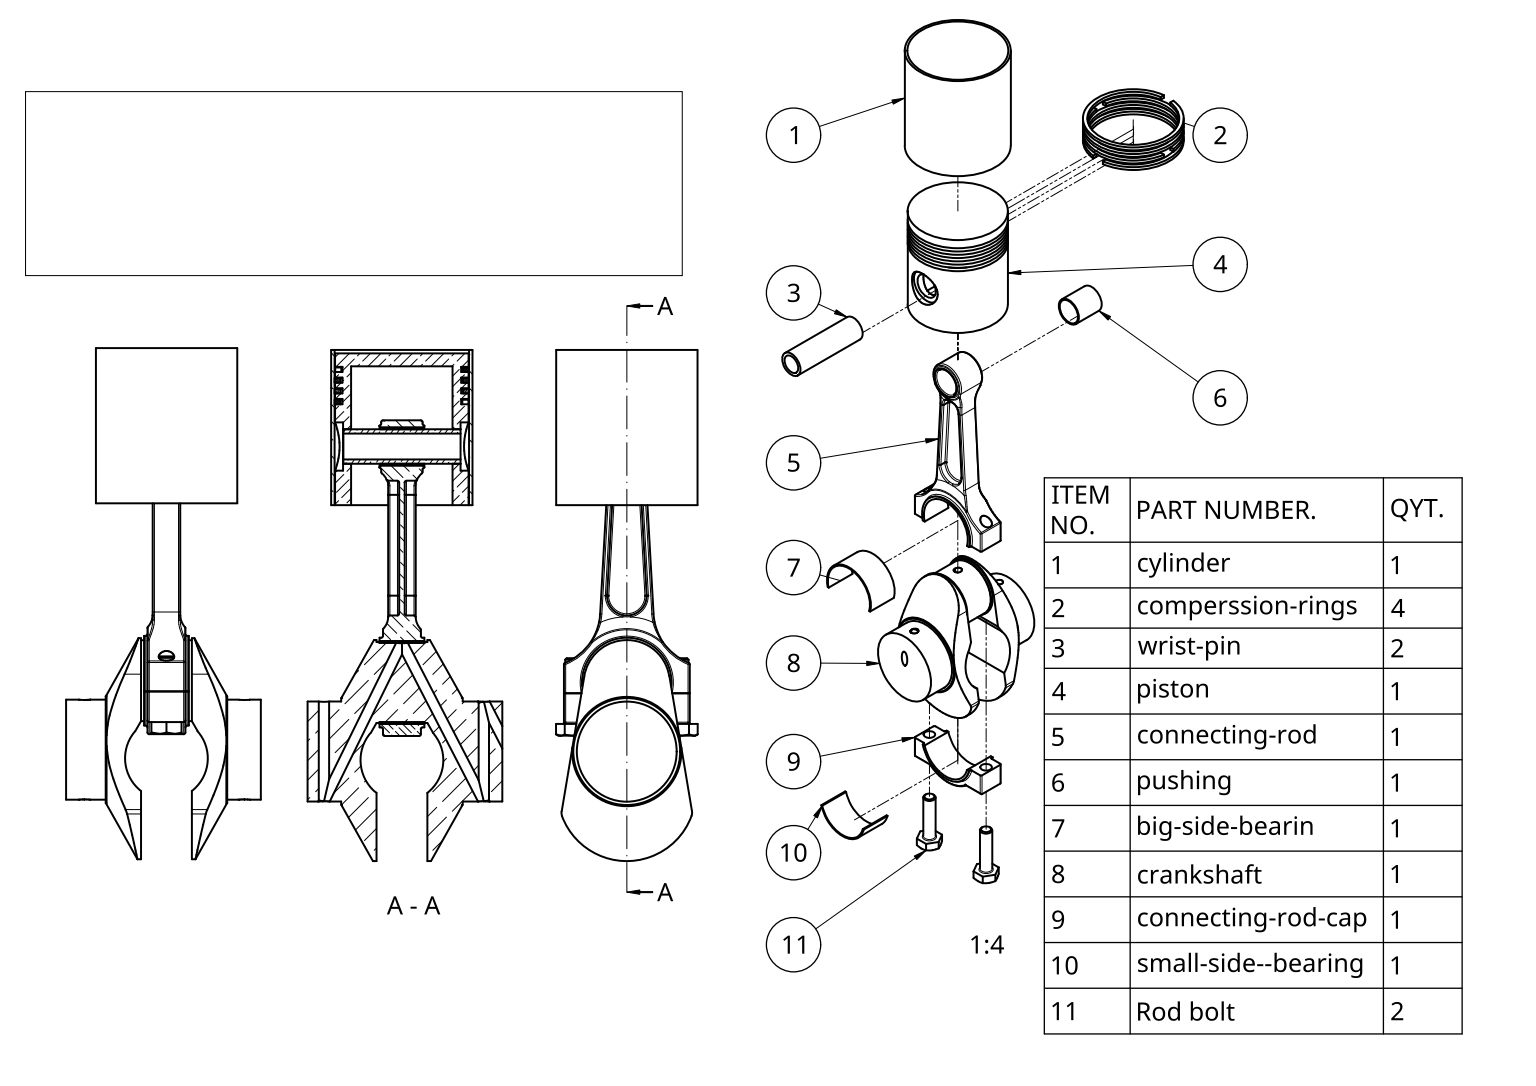
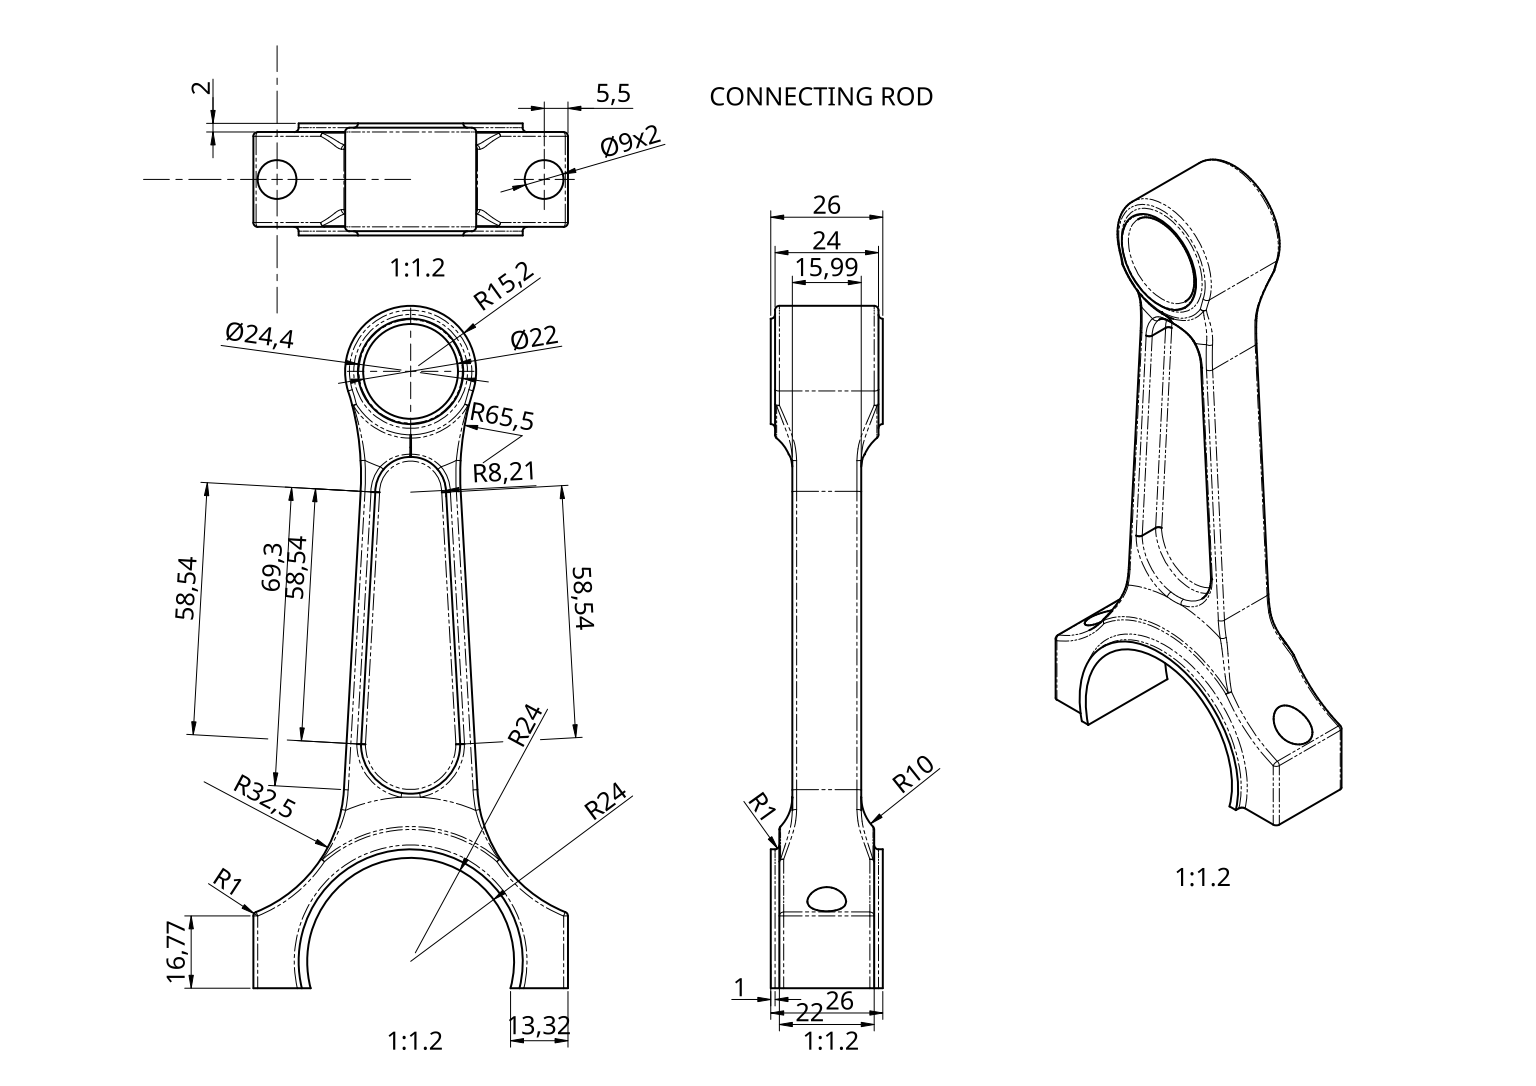
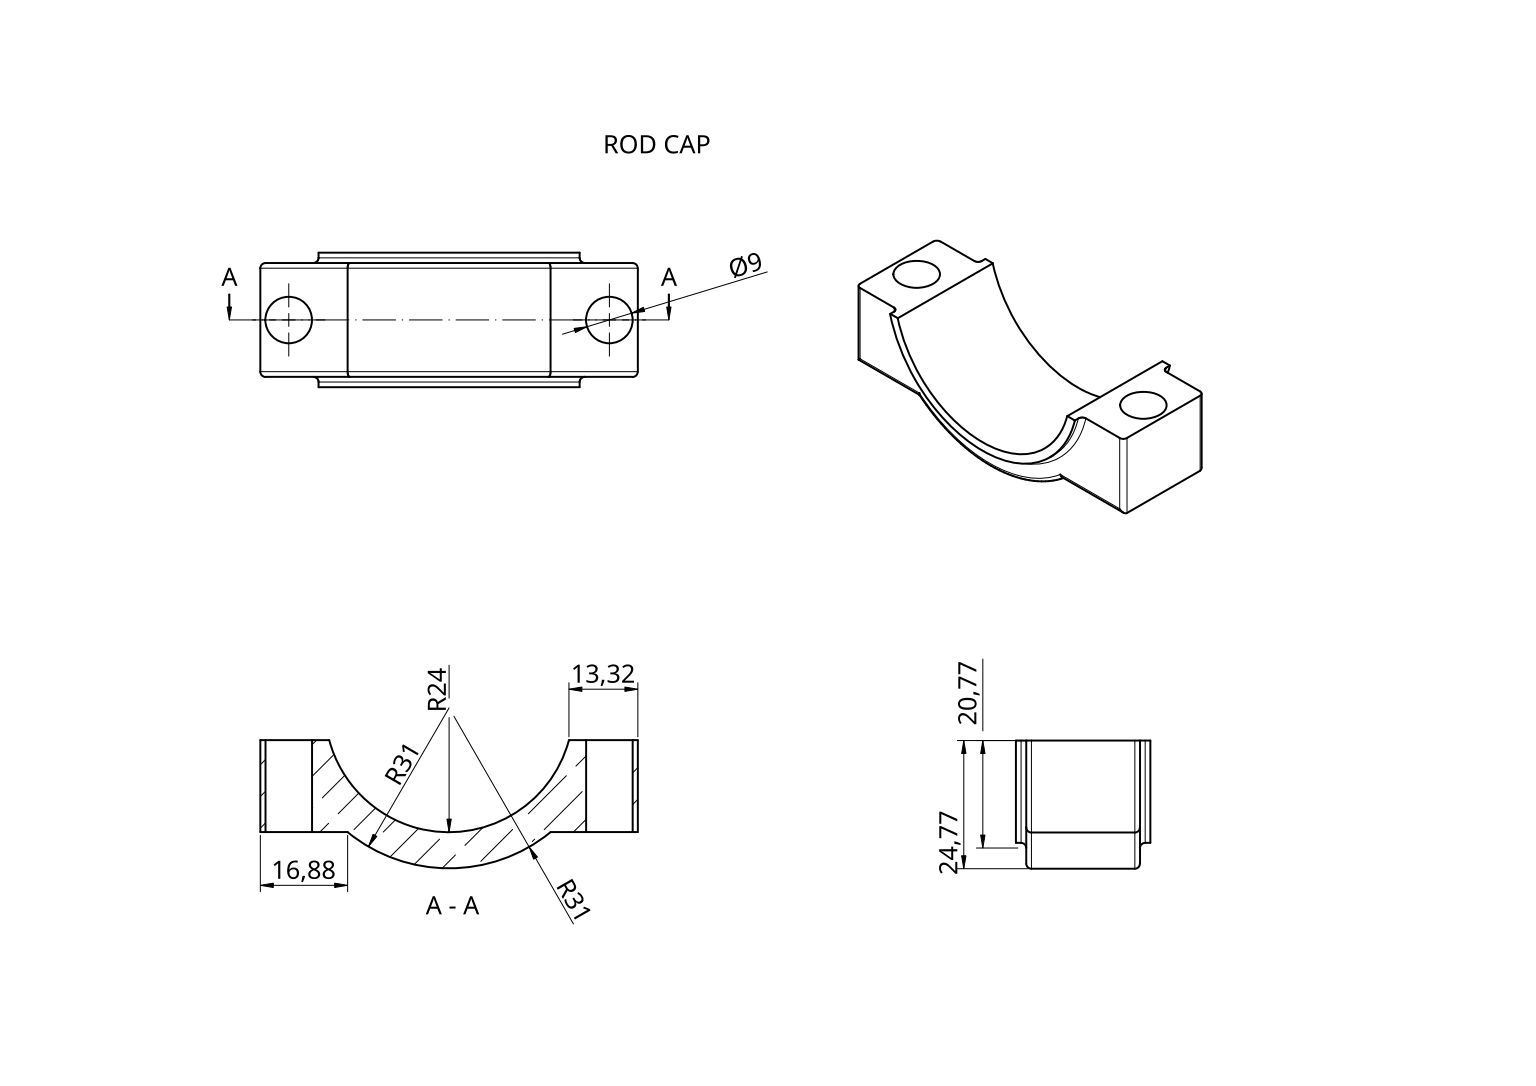
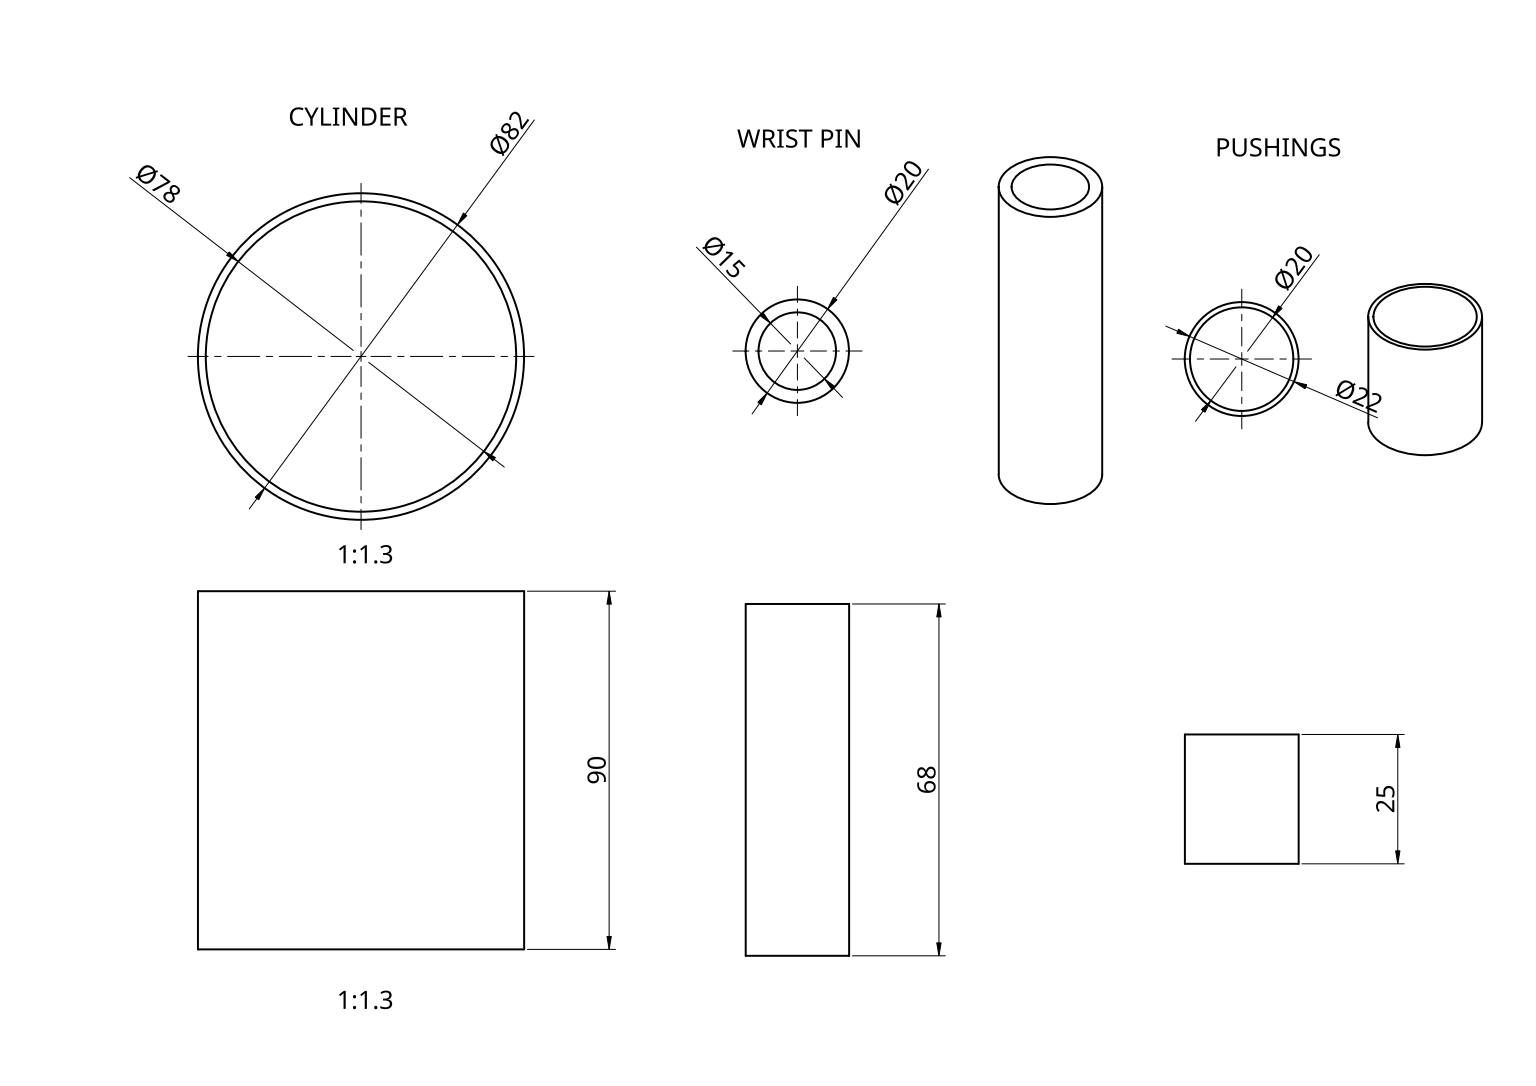
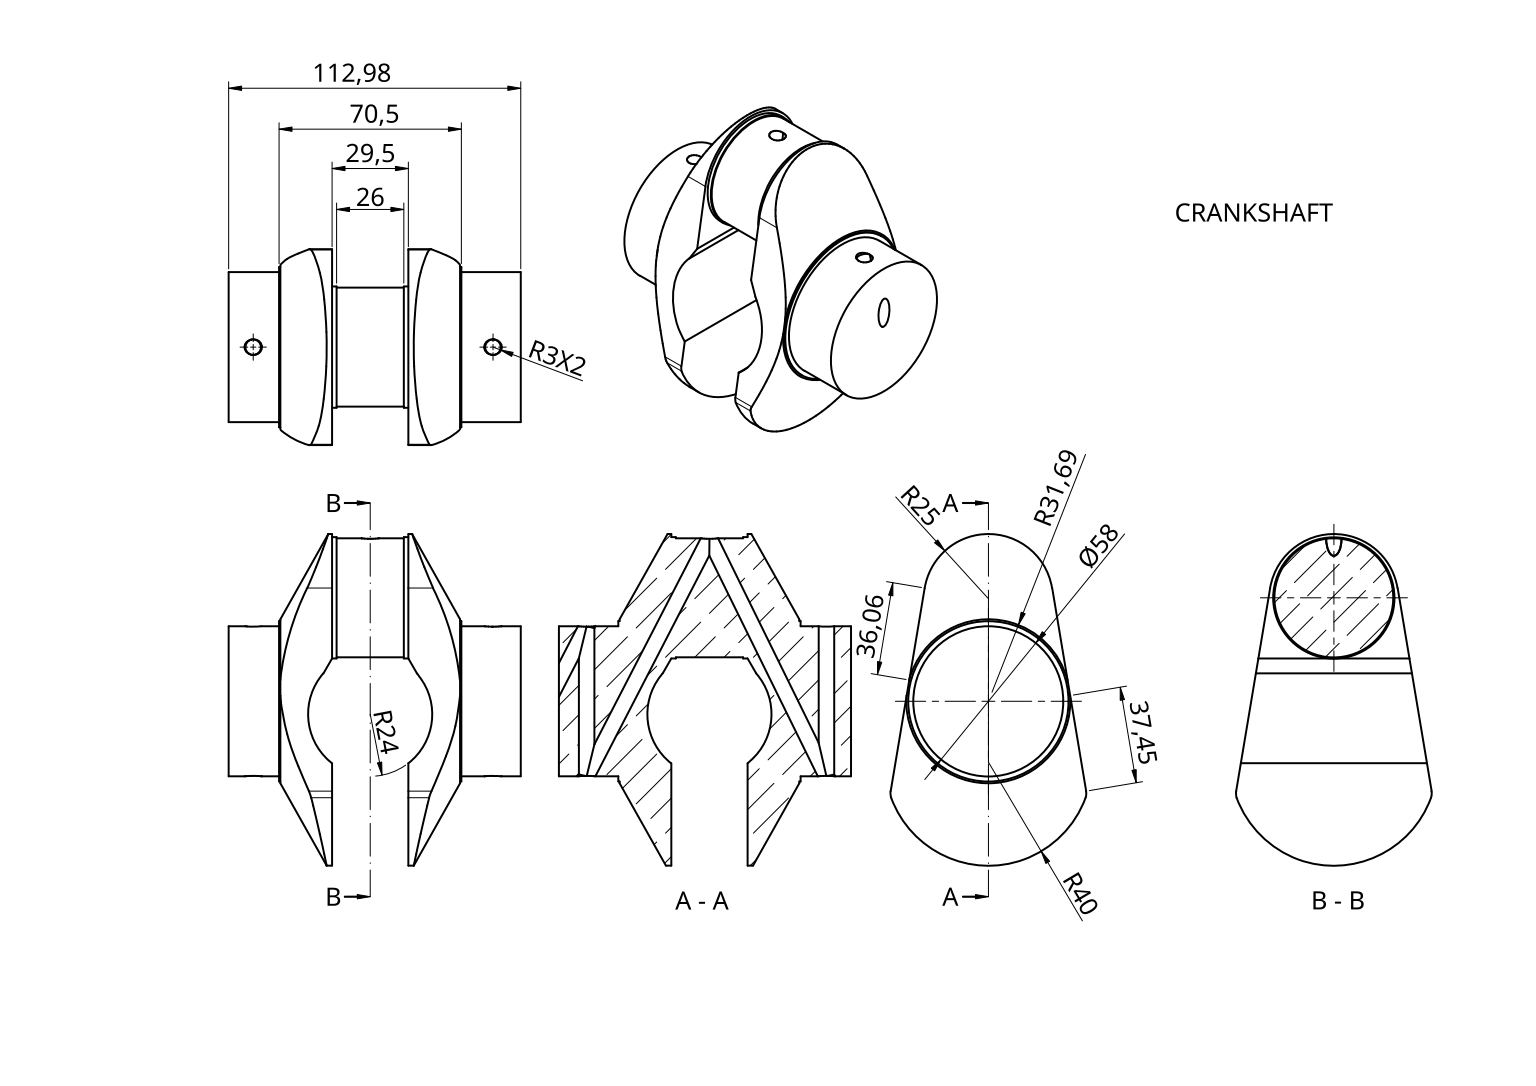
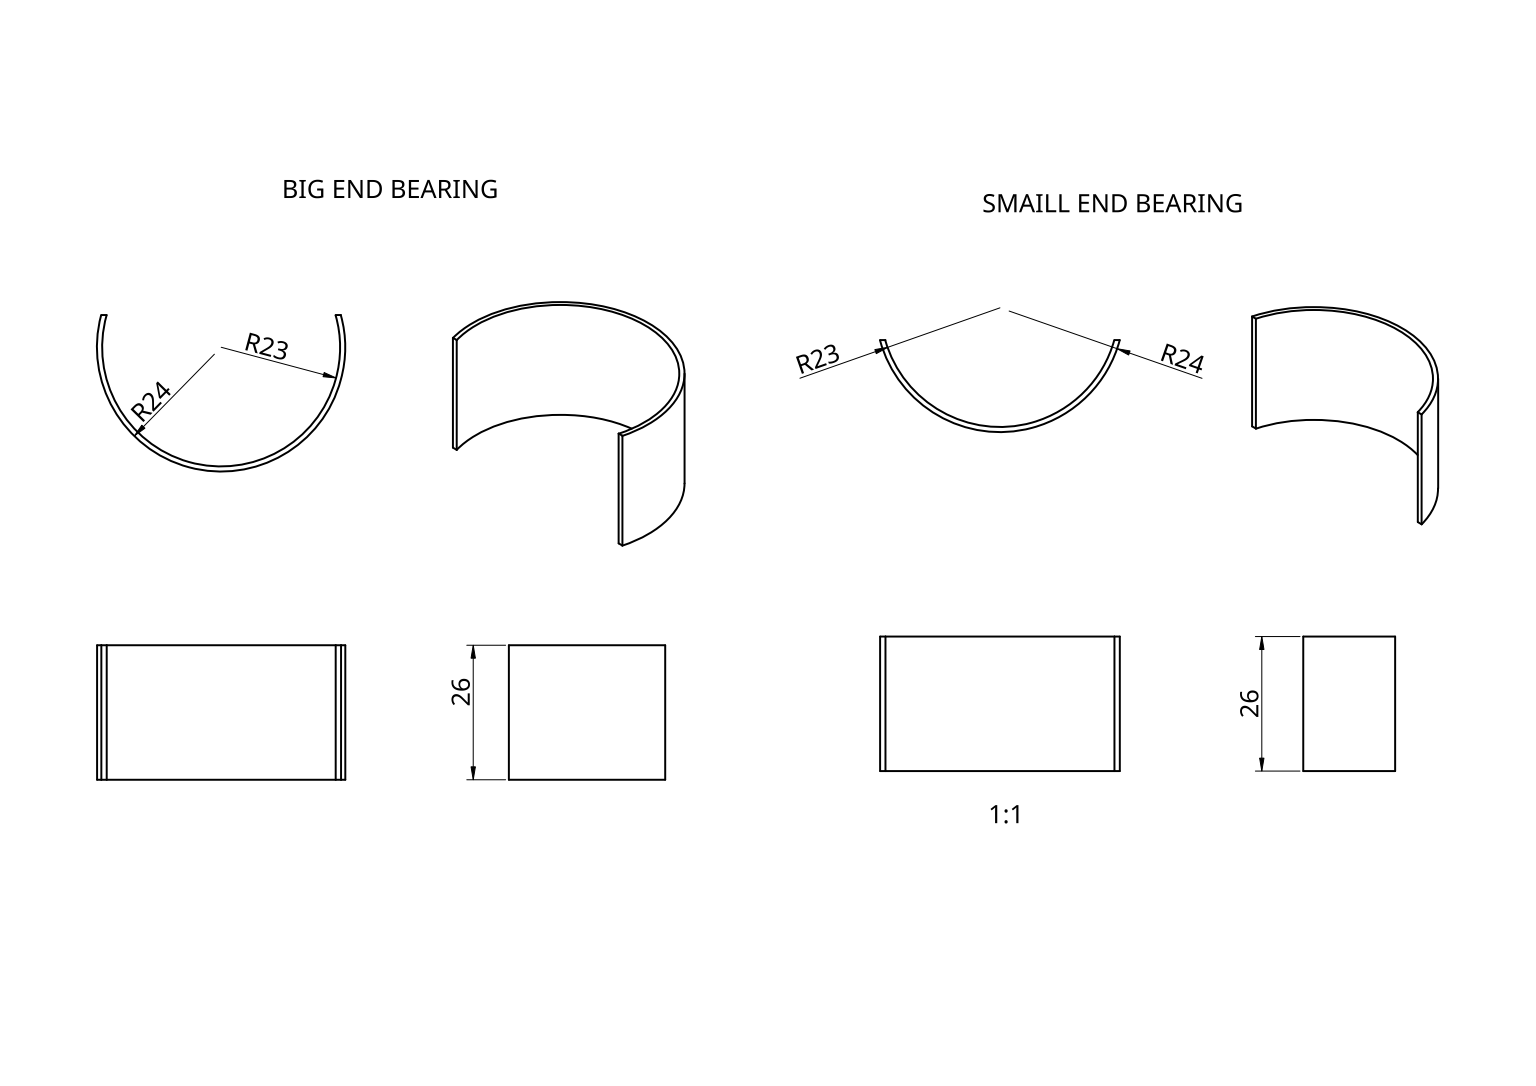
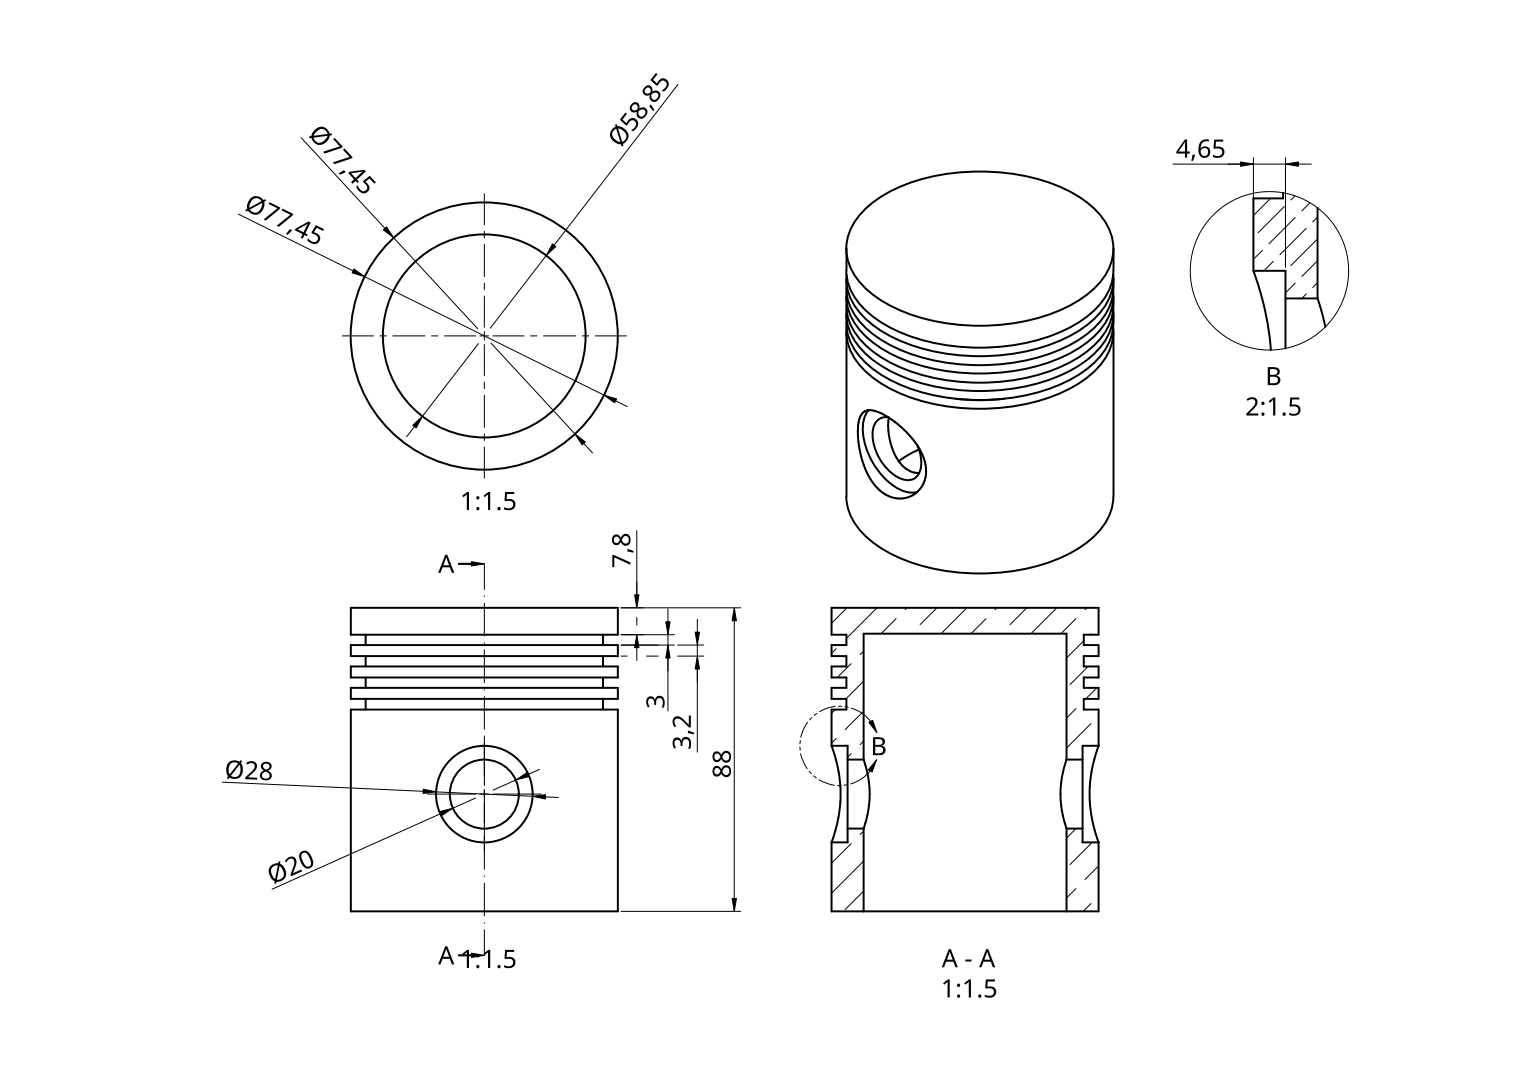
ISO-10303-21;
HEADER;
/* Generated by software containing ST-Developer
 * from STEP Tools, Inc. (www.steptools.com) 
 */
/* OPTION: using custom renumber hook */

FILE_DESCRIPTION(
/* description */ ('STEP AP242 Edition 2', 'CAx-IF Rec.Pracs.---Representation and Presentation of Product Manufa
cturing Information (PMI)---4.0---2014-10-13', 'CAx-IF Rec.Pracs.---3D Tessellated Geometry---0.4---2014-09-14', '2;1', 'CAx-IF Rec.Pracs.---User Defined Attributes---1.5---2016-08-15'),
/* implementation_level */ '2;1');

FILE_NAME(
/* name */ 'MAS-680',
/* time_stamp */ '2026-10-07T00:00:55Z',
/* author */ (''),
/* organization */ (''),
/* preprocessor_version */ 'ST-DEVELOPER v20',
/* originating_system */ 'ONSHAPE BY PTC INC, 1.221',
/* authorisation */ '  ');

FILE_SCHEMA (('AP242_MANAGED_MODEL_BASED_3D_ENGINEERING_MIM_LF { 1 0 10303 442 3 1 4 }'));
ENDSEC;

DATA;
#10=OVER_RIDING_STYLED_ITEM('',(#4355),#4278,#4343);
#11=OVER_RIDING_STYLED_ITEM('',(#4356),#4288,#4343);
#12=OVER_RIDING_STYLED_ITEM('',(#4357),#4289,#4343);
#13=OVER_RIDING_STYLED_ITEM('',(#4358),#4291,#4343);
#14=OVER_RIDING_STYLED_ITEM('',(#4359),#4293,#4343);
#15=SPHERICAL_SURFACE('',#4886,0.001);
#16=SPHERICAL_SURFACE('',#4890,0.001);
#17=SPHERICAL_SURFACE('',#4891,0.001);
#18=SPHERICAL_SURFACE('',#4895,0.001);
#19=SPHERICAL_SURFACE('',#4896,0.001);
#20=SPHERICAL_SURFACE('',#4900,0.001);
#21=SPHERICAL_SURFACE('',#4901,0.001);
#22=SPHERICAL_SURFACE('',#4905,0.001);
#23=SPHERICAL_SURFACE('',#4913,0.001);
#24=SPHERICAL_SURFACE('',#4915,0.001);
#25=SPHERICAL_SURFACE('',#4930,0.001);
#26=SPHERICAL_SURFACE('',#4932,0.001);
#27=(
BOUNDED_SURFACE()
B_SPLINE_SURFACE(3,2,((#7577,#7578,#7579),(#7580,#7581,#7582),(#7583,#7584,
#7585),(#7586,#7587,#7588)),.UNSPECIFIED.,.F.,.F.,.F.)
B_SPLINE_SURFACE_WITH_KNOTS((4,4),(3,3),(1.34441069388203E-17,0.00447796131591151),
(0.,1.),.PIECEWISE_BEZIER_KNOTS.)
GEOMETRIC_REPRESENTATION_ITEM()
RATIONAL_B_SPLINE_SURFACE(((1.,0.707106781186548,1.),(1.,0.71832066777653,
1.),(1.,0.718320667776528,1.),(1.,0.707106781186548,1.)))
REPRESENTATION_ITEM('')
SURFACE()
);
#28=(
BOUNDED_SURFACE()
B_SPLINE_SURFACE(3,2,((#7598,#7599,#7600),(#7601,#7602,#7603),(#7604,#7605,
#7606),(#7607,#7608,#7609),(#7610,#7611,#7612),(#7613,#7614,#7615)),
 .UNSPECIFIED.,.F.,.F.,.F.)
B_SPLINE_SURFACE_WITH_KNOTS((4,1,1,4),(3,3),(1.73472347597681E-18,0.00200651263897263,
0.00401302527794525,0.00802605055589049),(0.,1.),.UNSPECIFIED.)
GEOMETRIC_REPRESENTATION_ITEM()
RATIONAL_B_SPLINE_SURFACE(((1.,0.707106781186545,1.),(1.,0.714777484158914,
1.),(1.,0.738208449186217,1.),(1.,0.801379168437336,1.),(1.,0.836044012640875,
1.),(1.,0.836426120169544,1.)))
REPRESENTATION_ITEM('')
SURFACE()
);
#29=(
BOUNDED_SURFACE()
B_SPLINE_SURFACE(3,2,((#7635,#7636,#7637),(#7638,#7639,#7640),(#7641,#7642,
#7643),(#7644,#7645,#7646),(#7647,#7648,#7649),(#7650,#7651,#7652)),
 .UNSPECIFIED.,.F.,.F.,.F.)
B_SPLINE_SURFACE_WITH_KNOTS((4,1,1,4),(3,3),(-3.03576608295941E-18,0.00200651263897293,
0.00401302527794587,0.00802605055589175),(0.,1.),.UNSPECIFIED.)
GEOMETRIC_REPRESENTATION_ITEM()
RATIONAL_B_SPLINE_SURFACE(((1.,0.707106781186545,1.),(1.,0.714777484158915,
1.),(1.,0.738208449186387,1.),(1.,0.801379168436544,1.),(1.,0.836044012644433,
1.),(1.,0.836426120169542,1.)))
REPRESENTATION_ITEM('')
SURFACE()
);
#30=(
BOUNDED_SURFACE()
B_SPLINE_SURFACE(3,2,((#7656,#7657,#7658),(#7659,#7660,#7661),(#7662,#7663,
#7664),(#7665,#7666,#7667),(#7668,#7669,#7670)),.UNSPECIFIED.,.F.,.F.,.F.)
B_SPLINE_SURFACE_WITH_KNOTS((4,1,4),(3,3),(6.07153216591882E-18,0.00665411743559359,
0.0133082348711872),(0.,1.),.UNSPECIFIED.)
GEOMETRIC_REPRESENTATION_ITEM()
RATIONAL_B_SPLINE_SURFACE(((1.,0.707106781186547,1.),(1.,0.740921782108448,
1.),(1.,0.824106244556533,1.),(1.,0.890843705762328,1.),(1.,0.91150190641835,
1.)))
REPRESENTATION_ITEM('')
SURFACE()
);
#31=(
BOUNDED_SURFACE()
B_SPLINE_SURFACE(3,2,((#7679,#7680,#7681),(#7682,#7683,#7684),(#7685,#7686,
#7687),(#7688,#7689,#7690),(#7691,#7692,#7693),(#7694,#7695,#7696),(#7697,
#7698,#7699)),.UNSPECIFIED.,.F.,.F.,.F.)
B_SPLINE_SURFACE_WITH_KNOTS((4,1,1,1,4),(3,3),(1.21430643318376E-17,0.00345379209395837,
0.00690758418791672,0.0103613762818751,0.0138151683758334),(0.,1.),
 .UNSPECIFIED.)
GEOMETRIC_REPRESENTATION_ITEM()
RATIONAL_B_SPLINE_SURFACE(((1.,0.707106781186548,1.),(1.,0.723426406098682,
1.),(1.,0.760247481516635,1.),(1.,0.823847581524476,1.),(1.,0.886001526698892,
1.),(1.,0.919854499330898,1.),(1.,0.932470639919717,1.)))
REPRESENTATION_ITEM('')
SURFACE()
);
#32=(
BOUNDED_SURFACE()
B_SPLINE_SURFACE(3,2,((#7704,#7705,#7706),(#7707,#7708,#7709),(#7710,#7711,
#7712),(#7713,#7714,#7715),(#7716,#7717,#7718)),.UNSPECIFIED.,.F.,.F.,.F.)
B_SPLINE_SURFACE_WITH_KNOTS((4,1,4),(3,3),(6.07153216591882E-18,0.00665411743559357,
0.0133082348711871),(0.,1.),.UNSPECIFIED.)
GEOMETRIC_REPRESENTATION_ITEM()
RATIONAL_B_SPLINE_SURFACE(((1.,0.707106781186547,1.),(1.,0.740921782108448,
1.),(1.,0.824106244558266,1.),(1.,0.890843705758863,1.),(1.,0.91150190641835,
1.)))
REPRESENTATION_ITEM('')
SURFACE()
);
#33=(
BOUNDED_SURFACE()
B_SPLINE_SURFACE(3,2,((#7727,#7728,#7729),(#7730,#7731,#7732),(#7733,#7734,
#7735),(#7736,#7737,#7738),(#7739,#7740,#7741),(#7742,#7743,#7744),(#7745,
#7746,#7747)),.UNSPECIFIED.,.F.,.F.,.F.)
B_SPLINE_SURFACE_WITH_KNOTS((4,1,1,1,4),(3,3),(1.21430643318376E-17,0.00345379209395348,
0.00690758418790696,0.0103613762818604,0.0138151683758139),(0.,1.),
 .UNSPECIFIED.)
GEOMETRIC_REPRESENTATION_ITEM()
RATIONAL_B_SPLINE_SURFACE(((1.,0.707106781186548,1.),(1.,0.723426406098659,
1.),(1.,0.760247481516514,1.),(1.,0.823847581524435,1.),(1.,0.88600152669811,
1.),(1.,0.919854499331796,1.),(1.,0.932470639919502,1.)))
REPRESENTATION_ITEM('')
SURFACE()
);
#34=(
BOUNDED_SURFACE()
B_SPLINE_SURFACE(3,2,((#7762,#7763,#7764),(#7765,#7766,#7767),(#7768,#7769,
#7770),(#7771,#7772,#7773)),.UNSPECIFIED.,.F.,.F.,.F.)
B_SPLINE_SURFACE_WITH_KNOTS((4,4),(3,3),(-6.07153216591882E-18,0.00447796131591189),
(0.,1.),.PIECEWISE_BEZIER_KNOTS.)
GEOMETRIC_REPRESENTATION_ITEM()
RATIONAL_B_SPLINE_SURFACE(((1.,0.707106781186547,1.),(1.,0.718320667778804,
1.),(1.,0.718320667774086,1.),(1.,0.707106781186547,1.)))
REPRESENTATION_ITEM('')
SURFACE()
);
#35=(
BOUNDED_SURFACE()
B_SPLINE_SURFACE(3,2,((#7783,#7784,#7785),(#7786,#7787,#7788),(#7789,#7790,
#7791),(#7792,#7793,#7794),(#7795,#7796,#7797),(#7798,#7799,#7800)),
 .UNSPECIFIED.,.F.,.F.,.F.)
B_SPLINE_SURFACE_WITH_KNOTS((4,1,1,4),(3,3),(-6.07153216591882E-18,0.00200651263897325,
0.00401302527794651,0.00802605055589303),(0.,1.),.UNSPECIFIED.)
GEOMETRIC_REPRESENTATION_ITEM()
RATIONAL_B_SPLINE_SURFACE(((1.,0.707106781186545,1.),(1.,0.71477748415869,
1.),(1.,0.738208449186489,1.),(1.,0.801379168436508,1.),(1.,0.836044012644435,
1.),(1.,0.836426120169544,1.)))
REPRESENTATION_ITEM('')
SURFACE()
);
#36=(
BOUNDED_SURFACE()
B_SPLINE_SURFACE(3,2,((#7820,#7821,#7822),(#7823,#7824,#7825),(#7826,#7827,
#7828),(#7829,#7830,#7831),(#7832,#7833,#7834),(#7835,#7836,#7837)),
 .UNSPECIFIED.,.F.,.F.,.F.)
B_SPLINE_SURFACE_WITH_KNOTS((4,1,1,4),(3,3),(-3.46944695195361E-18,0.00200651263897327,
0.00401302527794655,0.0080260505558931),(0.,1.),.UNSPECIFIED.)
GEOMETRIC_REPRESENTATION_ITEM()
RATIONAL_B_SPLINE_SURFACE(((1.,0.707106781186545,1.),(1.,0.71477748415869,
1.),(1.,0.738208449186491,1.),(1.,0.80137916843651,1.),(1.,0.836044012644435,
1.),(1.,0.836426120169544,1.)))
REPRESENTATION_ITEM('')
SURFACE()
);
#37=(
BOUNDED_SURFACE()
B_SPLINE_SURFACE(3,2,((#7841,#7842,#7843),(#7844,#7845,#7846),(#7847,#7848,
#7849),(#7850,#7851,#7852),(#7853,#7854,#7855)),.UNSPECIFIED.,.F.,.F.,.F.)
B_SPLINE_SURFACE_WITH_KNOTS((4,1,4),(3,3),(-1.90819582357449E-17,0.00665411743559197,
0.013308234871184),(0.,1.),.UNSPECIFIED.)
GEOMETRIC_REPRESENTATION_ITEM()
RATIONAL_B_SPLINE_SURFACE(((1.,0.707106781186595,1.),(1.,0.740921782104245,
1.),(1.,0.824106244558438,1.),(1.,0.890843705762829,1.),(1.,0.911501906418351,
1.)))
REPRESENTATION_ITEM('')
SURFACE()
);
#38=(
BOUNDED_SURFACE()
B_SPLINE_SURFACE(3,2,((#7864,#7865,#7866),(#7867,#7868,#7869),(#7870,#7871,
#7872),(#7873,#7874,#7875),(#7876,#7877,#7878),(#7879,#7880,#7881),(#7882,
#7883,#7884)),.UNSPECIFIED.,.F.,.F.,.F.)
B_SPLINE_SURFACE_WITH_KNOTS((4,1,1,1,4),(3,3),(1.99493199737333E-17,0.00345379209395838,
0.00690758418791674,0.0103613762818751,0.0138151683758335),(0.,1.),
 .UNSPECIFIED.)
GEOMETRIC_REPRESENTATION_ITEM()
RATIONAL_B_SPLINE_SURFACE(((1.,0.707106781186548,1.),(1.,0.723426406098682,
1.),(1.,0.760247481516625,1.),(1.,0.823847581524508,1.),(1.,0.886001526698772,
1.),(1.,0.919854499331156,1.),(1.,0.932470639919717,1.)))
REPRESENTATION_ITEM('')
SURFACE()
);
#39=(
BOUNDED_SURFACE()
B_SPLINE_SURFACE(3,2,((#7889,#7890,#7891),(#7892,#7893,#7894),(#7895,#7896,
#7897),(#7898,#7899,#7900),(#7901,#7902,#7903)),.UNSPECIFIED.,.F.,.F.,.F.)
B_SPLINE_SURFACE_WITH_KNOTS((4,1,4),(3,3),(5.20417042793042E-18,0.0066541174355936,
0.0133082348711872),(0.,1.),.UNSPECIFIED.)
GEOMETRIC_REPRESENTATION_ITEM()
RATIONAL_B_SPLINE_SURFACE(((1.,0.707106781186548,1.),(1.,0.740921782105829,
1.),(1.,0.824106244557286,1.),(1.,0.890843705763443,1.),(1.,0.911501906418351,
1.)))
REPRESENTATION_ITEM('')
SURFACE()
);
#40=(
BOUNDED_SURFACE()
B_SPLINE_SURFACE(3,2,((#7912,#7913,#7914),(#7915,#7916,#7917),(#7918,#7919,
#7920),(#7921,#7922,#7923),(#7924,#7925,#7926),(#7927,#7928,#7929),(#7930,
#7931,#7932)),.UNSPECIFIED.,.F.,.F.,.F.)
B_SPLINE_SURFACE_WITH_KNOTS((4,1,1,1,4),(3,3),(8.67361737988404E-18,0.00345379209395273,
0.00690758418790545,0.0103613762818582,0.0138151683758109),(0.,1.),
 .UNSPECIFIED.)
GEOMETRIC_REPRESENTATION_ITEM()
RATIONAL_B_SPLINE_SURFACE(((1.,0.707106781186591,1.),(1.,0.723426406097336,
1.),(1.,0.760247481517187,1.),(1.,0.823847581524302,1.),(1.,0.886001526698139,
1.),(1.,0.919854499331863,1.),(1.,0.932470639919503,1.)))
REPRESENTATION_ITEM('')
SURFACE()
);
#41=ELLIPSE('',#4605,0.00141421356237309,0.001);
#42=ELLIPSE('',#4607,0.00141421356237309,0.001);
#43=ELLIPSE('',#4609,0.00141421356237309,0.001);
#44=ELLIPSE('',#4611,0.00141421356237309,0.001);
#45=ELLIPSE('',#4974,0.0243340224134753,0.023999999999999);
#46=ELLIPSE('',#4977,0.0243340224134761,0.024000000000001);
#47=ELLIPSE('',#4992,0.00666547755067305,0.00299999999999906);
#48=ELLIPSE('',#4993,0.0127089644991076,0.00300000000000008);
#49=ELLIPSE('',#4995,0.0132410741485331,0.00299999999999985);
#50=ELLIPSE('',#5007,0.00308724563751592,0.003);
#51=ELLIPSE('',#5008,0.0127089644991094,0.00300000000000053);
#52=ELLIPSE('',#5009,0.00308724563751592,0.003);
#53=ELLIPSE('',#5015,0.00308009663615096,0.003);
#54=ELLIPSE('',#5024,0.00653928253453561,0.003);
#55=ELLIPSE('',#5027,0.0243340224134758,0.0240000000000003);
#56=ELLIPSE('',#5030,0.0243340224134756,0.0239999999999998);
#57=CONTEXT_DEPENDENT_SHAPE_REPRESENTATION(#87,#8564);
#58=CONTEXT_DEPENDENT_SHAPE_REPRESENTATION(#88,#8566);
#59=CONTEXT_DEPENDENT_SHAPE_REPRESENTATION(#89,#8568);
#60=CONTEXT_DEPENDENT_SHAPE_REPRESENTATION(#90,#8570);
#61=CONTEXT_DEPENDENT_SHAPE_REPRESENTATION(#91,#8571);
#62=CONTEXT_DEPENDENT_SHAPE_REPRESENTATION(#92,#8572);
#63=CONTEXT_DEPENDENT_SHAPE_REPRESENTATION(#93,#8574);
#64=CONTEXT_DEPENDENT_SHAPE_REPRESENTATION(#94,#8576);
#65=CONTEXT_DEPENDENT_SHAPE_REPRESENTATION(#95,#8577);
#66=CONTEXT_DEPENDENT_SHAPE_REPRESENTATION(#96,#8579);
#67=CONTEXT_DEPENDENT_SHAPE_REPRESENTATION(#97,#8581);
#68=CONTEXT_DEPENDENT_SHAPE_REPRESENTATION(#98,#8583);
#69=CONTEXT_DEPENDENT_SHAPE_REPRESENTATION(#99,#8585);
#70=CONTEXT_DEPENDENT_SHAPE_REPRESENTATION(#100,#8587);
#71=CONTEXT_DEPENDENT_SHAPE_REPRESENTATION(#101,#8588);
#72=NEXT_ASSEMBLY_USAGE_OCCURRENCE('NAUO1',
'Heavy hex bolt 3/8-16 x 1.5','Heavy hex bolt 3/8-16 x 1.5',#8589,#8590,
'');
#73=NEXT_ASSEMBLY_USAGE_OCCURRENCE('NAUO2','Part 1','Part 1',#8589,#8591,
'');
#74=NEXT_ASSEMBLY_USAGE_OCCURRENCE('NAUO3','Part 1','Part 1',#8589,#8592,
'');
#75=NEXT_ASSEMBLY_USAGE_OCCURRENCE('NAUO4','Part 1','Part 1',#8589,#8593,
'');
#76=NEXT_ASSEMBLY_USAGE_OCCURRENCE('NAUO5','Part 1','Part 1',#8589,#8592,
'');
#77=NEXT_ASSEMBLY_USAGE_OCCURRENCE('NAUO6',
'Heavy hex bolt 3/8-16 x 1.5','Heavy hex bolt 3/8-16 x 1.5',#8589,#8590,
'');
#78=NEXT_ASSEMBLY_USAGE_OCCURRENCE('NAUO7','Part 1','Part 1',#8589,#8594,
'');
#79=NEXT_ASSEMBLY_USAGE_OCCURRENCE('NAUO8','Part 2','Part 2',#8589,#8595,
'');
#80=NEXT_ASSEMBLY_USAGE_OCCURRENCE('NAUO9','Part 1','Part 1',#8589,#8592,
'');
#81=NEXT_ASSEMBLY_USAGE_OCCURRENCE('NAUO10','Part 1','Part 1',#8589,#8596,
'');
#82=NEXT_ASSEMBLY_USAGE_OCCURRENCE('NAUO11','Part 4','Part 4',#8589,#8597,
'');
#83=NEXT_ASSEMBLY_USAGE_OCCURRENCE('NAUO12','Part 2','Part 2',#8589,#8598,
'');
#84=NEXT_ASSEMBLY_USAGE_OCCURRENCE('NAUO13','CRANKSHAFT','CRANKSHAFT',#8589,
#8599,'');
#85=NEXT_ASSEMBLY_USAGE_OCCURRENCE('NAUO14','Part 3','Part 3',#8589,#8600,
'');
#86=NEXT_ASSEMBLY_USAGE_OCCURRENCE('NAUO15','Part 1','Part 1',#8589,#8592,
'');
#87=(
REPRESENTATION_RELATIONSHIP(' ',' ',#4473,#4472)
REPRESENTATION_RELATIONSHIP_WITH_TRANSFORMATION(#102)
SHAPE_REPRESENTATION_RELATIONSHIP()
);
#88=(
REPRESENTATION_RELATIONSHIP(' ',' ',#4474,#4472)
REPRESENTATION_RELATIONSHIP_WITH_TRANSFORMATION(#103)
SHAPE_REPRESENTATION_RELATIONSHIP()
);
#89=(
REPRESENTATION_RELATIONSHIP(' ',' ',#4475,#4472)
REPRESENTATION_RELATIONSHIP_WITH_TRANSFORMATION(#104)
SHAPE_REPRESENTATION_RELATIONSHIP()
);
#90=(
REPRESENTATION_RELATIONSHIP(' ',' ',#4476,#4472)
REPRESENTATION_RELATIONSHIP_WITH_TRANSFORMATION(#105)
SHAPE_REPRESENTATION_RELATIONSHIP()
);
#91=(
REPRESENTATION_RELATIONSHIP(' ',' ',#4475,#4472)
REPRESENTATION_RELATIONSHIP_WITH_TRANSFORMATION(#106)
SHAPE_REPRESENTATION_RELATIONSHIP()
);
#92=(
REPRESENTATION_RELATIONSHIP(' ',' ',#4473,#4472)
REPRESENTATION_RELATIONSHIP_WITH_TRANSFORMATION(#107)
SHAPE_REPRESENTATION_RELATIONSHIP()
);
#93=(
REPRESENTATION_RELATIONSHIP(' ',' ',#4477,#4472)
REPRESENTATION_RELATIONSHIP_WITH_TRANSFORMATION(#108)
SHAPE_REPRESENTATION_RELATIONSHIP()
);
#94=(
REPRESENTATION_RELATIONSHIP(' ',' ',#4478,#4472)
REPRESENTATION_RELATIONSHIP_WITH_TRANSFORMATION(#109)
SHAPE_REPRESENTATION_RELATIONSHIP()
);
#95=(
REPRESENTATION_RELATIONSHIP(' ',' ',#4475,#4472)
REPRESENTATION_RELATIONSHIP_WITH_TRANSFORMATION(#110)
SHAPE_REPRESENTATION_RELATIONSHIP()
);
#96=(
REPRESENTATION_RELATIONSHIP(' ',' ',#4479,#4472)
REPRESENTATION_RELATIONSHIP_WITH_TRANSFORMATION(#111)
SHAPE_REPRESENTATION_RELATIONSHIP()
);
#97=(
REPRESENTATION_RELATIONSHIP(' ',' ',#4480,#4472)
REPRESENTATION_RELATIONSHIP_WITH_TRANSFORMATION(#112)
SHAPE_REPRESENTATION_RELATIONSHIP()
);
#98=(
REPRESENTATION_RELATIONSHIP(' ',' ',#4481,#4472)
REPRESENTATION_RELATIONSHIP_WITH_TRANSFORMATION(#113)
SHAPE_REPRESENTATION_RELATIONSHIP()
);
#99=(
REPRESENTATION_RELATIONSHIP(' ',' ',#4482,#4472)
REPRESENTATION_RELATIONSHIP_WITH_TRANSFORMATION(#114)
SHAPE_REPRESENTATION_RELATIONSHIP()
);
#100=(
REPRESENTATION_RELATIONSHIP(' ',' ',#4483,#4472)
REPRESENTATION_RELATIONSHIP_WITH_TRANSFORMATION(#115)
SHAPE_REPRESENTATION_RELATIONSHIP()
);
#101=(
REPRESENTATION_RELATIONSHIP(' ',' ',#4475,#4472)
REPRESENTATION_RELATIONSHIP_WITH_TRANSFORMATION(#116)
SHAPE_REPRESENTATION_RELATIONSHIP()
);
#102=ITEM_DEFINED_TRANSFORMATION(' ',' ',#4484,#4513);
#103=ITEM_DEFINED_TRANSFORMATION(' ',' ',#4484,#4522);
#104=ITEM_DEFINED_TRANSFORMATION(' ',' ',#4484,#4533);
#105=ITEM_DEFINED_TRANSFORMATION(' ',' ',#4484,#4585);
#106=ITEM_DEFINED_TRANSFORMATION(' ',' ',#4484,#4586);
#107=ITEM_DEFINED_TRANSFORMATION(' ',' ',#4484,#4587);
#108=ITEM_DEFINED_TRANSFORMATION(' ',' ',#4484,#4596);
#109=ITEM_DEFINED_TRANSFORMATION(' ',' ',#4484,#4649);
#110=ITEM_DEFINED_TRANSFORMATION(' ',' ',#4484,#4650);
#111=ITEM_DEFINED_TRANSFORMATION(' ',' ',#4484,#4940);
#112=ITEM_DEFINED_TRANSFORMATION(' ',' ',#4484,#4951);
#113=ITEM_DEFINED_TRANSFORMATION(' ',' ',#4484,#4960);
#114=ITEM_DEFINED_TRANSFORMATION(' ',' ',#4484,#5051);
#115=ITEM_DEFINED_TRANSFORMATION(' ',' ',#4484,#5062);
#116=ITEM_DEFINED_TRANSFORMATION(' ',' ',#4484,#5063);
#117=SHAPE_REPRESENTATION_RELATIONSHIP('','',#4473,#128);
#118=SHAPE_REPRESENTATION_RELATIONSHIP('','',#4474,#129);
#119=SHAPE_REPRESENTATION_RELATIONSHIP('','',#4475,#130);
#120=SHAPE_REPRESENTATION_RELATIONSHIP('','',#4476,#131);
#121=SHAPE_REPRESENTATION_RELATIONSHIP('','',#4477,#132);
#122=SHAPE_REPRESENTATION_RELATIONSHIP('','',#4478,#133);
#123=SHAPE_REPRESENTATION_RELATIONSHIP('','',#4479,#134);
#124=SHAPE_REPRESENTATION_RELATIONSHIP('','',#4480,#135);
#125=SHAPE_REPRESENTATION_RELATIONSHIP('','',#4481,#136);
#126=SHAPE_REPRESENTATION_RELATIONSHIP('','',#4482,#137);
#127=SHAPE_REPRESENTATION_RELATIONSHIP('','',#4483,#138);
#128=ADVANCED_BREP_SHAPE_REPRESENTATION('',(#4449),#8536);
#129=ADVANCED_BREP_SHAPE_REPRESENTATION('',(#4450),#8537);
#130=ADVANCED_BREP_SHAPE_REPRESENTATION('',(#4451),#8538);
#131=ADVANCED_BREP_SHAPE_REPRESENTATION('',(#4452),#8539);
#132=ADVANCED_BREP_SHAPE_REPRESENTATION('',(#4453),#8540);
#133=ADVANCED_BREP_SHAPE_REPRESENTATION('',(#4454),#8541);
#134=ADVANCED_BREP_SHAPE_REPRESENTATION('',(#4455),#8542);
#135=ADVANCED_BREP_SHAPE_REPRESENTATION('',(#4456),#8543);
#136=ADVANCED_BREP_SHAPE_REPRESENTATION('',(#4457),#8544);
#137=ADVANCED_BREP_SHAPE_REPRESENTATION('',(#4458),#8545);
#138=ADVANCED_BREP_SHAPE_REPRESENTATION('',(#4459),#8546);
#139=TOROIDAL_SURFACE('',#4511,0.0055245,0.000762);
#140=TOROIDAL_SURFACE('',#4600,0.03,0.001);
#141=TOROIDAL_SURFACE('',#4602,0.03,0.001);
#142=TOROIDAL_SURFACE('',#4620,0.027,0.001);
#143=TOROIDAL_SURFACE('',#4624,0.027,0.001);
#144=TOROIDAL_SURFACE('',#4690,0.027,0.001);
#145=TOROIDAL_SURFACE('',#4691,0.027,0.001);
#146=TOROIDAL_SURFACE('',#4788,0.0232046666802154,0.01);
#147=TOROIDAL_SURFACE('',#4791,0.0232046666802154,0.01);
#148=TOROIDAL_SURFACE('',#4793,0.0232046666802154,0.01);
#149=TOROIDAL_SURFACE('',#4796,0.0232046666802154,0.01);
#150=TOROIDAL_SURFACE('',#4798,0.0381475271495645,0.01);
#151=TOROIDAL_SURFACE('',#4800,0.0381475271495645,0.01);
#152=TOROIDAL_SURFACE('',#4802,0.0104910488,0.001);
#153=TOROIDAL_SURFACE('',#4805,0.007207892,0.001);
#154=TOROIDAL_SURFACE('',#4812,0.0124910488,0.001);
#155=TOROIDAL_SURFACE('',#4816,0.009207892,0.001);
#156=TOROIDAL_SURFACE('',#4818,0.0124910488,0.001);
#157=TOROIDAL_SURFACE('',#4821,0.009207892,0.001);
#158=TOROIDAL_SURFACE('',#4823,0.0335028673605553,0.001);
#159=TOROIDAL_SURFACE('',#4828,0.0335028673605553,0.001);
#160=TOROIDAL_SURFACE('',#4832,0.0665016995023668,0.001);
#161=TOROIDAL_SURFACE('',#4835,0.0335028673605553,0.001);
#162=TOROIDAL_SURFACE('',#4840,0.0335028673605553,0.001);
#163=TOROIDAL_SURFACE('',#4844,0.0665016995023668,0.001);
#164=TOROIDAL_SURFACE('',#4847,0.0124910488,0.001);
#165=TOROIDAL_SURFACE('',#4851,0.009207892,0.001);
#166=TOROIDAL_SURFACE('',#4853,0.0124910488,0.001);
#167=TOROIDAL_SURFACE('',#4855,0.0174510516898875,0.0164511617441065);
#168=TOROIDAL_SURFACE('',#4856,0.009207892,0.001);
#169=TOROIDAL_SURFACE('',#4858,0.0335028673605553,0.001);
#170=TOROIDAL_SURFACE('',#4863,0.0335028673605553,0.001);
#171=TOROIDAL_SURFACE('',#4867,0.0665016995023668,0.001);
#172=TOROIDAL_SURFACE('',#4870,0.0335028673605553,0.001);
#173=TOROIDAL_SURFACE('',#4875,0.0335028673605553,0.001);
#174=TOROIDAL_SURFACE('',#4879,0.0665016995023668,0.001);
#175=TOROIDAL_SURFACE('',#4882,0.007207892,0.001);
#176=TOROIDAL_SURFACE('',#4885,0.0104910488,0.001);
#177=TOROIDAL_SURFACE('',#4888,0.030591099482527,0.001);
#178=TOROIDAL_SURFACE('',#4903,0.030591099482527,0.001);
#179=TOROIDAL_SURFACE('',#4906,0.0141998,0.001);
#180=TOROIDAL_SURFACE('',#4909,0.0665016995023668,0.001);
#181=TOROIDAL_SURFACE('',#4911,0.0665016995023668,0.001);
#182=TOROIDAL_SURFACE('',#4917,0.0147142518944256,0.001);
#183=TOROIDAL_SURFACE('',#4918,0.0147142518944256,0.001);
#184=TOROIDAL_SURFACE('',#4920,0.0132,0.001);
#185=TOROIDAL_SURFACE('',#4921,0.012,0.001);
#186=TOROIDAL_SURFACE('',#4922,0.012,0.001);
#187=TOROIDAL_SURFACE('',#4923,0.0141998,0.001);
#188=TOROIDAL_SURFACE('',#4926,0.0665016995023668,0.001);
#189=TOROIDAL_SURFACE('',#4928,0.0665016995023668,0.001);
#190=TOROIDAL_SURFACE('',#4934,0.0147142518944256,0.001);
#191=TOROIDAL_SURFACE('',#4935,0.0147142518944256,0.001);
#192=TOROIDAL_SURFACE('',#4937,0.0132,0.001);
#193=CONICAL_SURFACE('',#4498,0.0087376,1.0471975511966);
#194=CONICAL_SURFACE('',#4500,0.0087376,1.0471975511966);
#195=CONICAL_SURFACE('',#4502,0.0087376,1.0471975511966);
#196=CONICAL_SURFACE('',#4504,0.0087376,1.0471975511966);
#197=CONICAL_SURFACE('',#4506,0.0087376,1.0471975511966);
#198=CONICAL_SURFACE('',#4508,0.0087376,1.0471975511966);
#199=CONICAL_SURFACE('',#4512,0.0039032404234375,0.785398163397448);
#200=CONICAL_SURFACE('',#4988,0.001,1.05851587994953);
#201=CONICAL_SURFACE('',#4989,0.001,1.05851587994953);
#202=CONICAL_SURFACE('',#5040,0.001,1.05851587994953);
#203=CONICAL_SURFACE('',#5044,0.001,1.05851587994953);
#204=CYLINDRICAL_SURFACE('',#4493,0.0047625);
#205=CYLINDRICAL_SURFACE('',#4520,0.041);
#206=CYLINDRICAL_SURFACE('',#4521,0.039);
#207=CYLINDRICAL_SURFACE('',#4523,0.039);
#208=CYLINDRICAL_SURFACE('',#4527,0.0355);
#209=CYLINDRICAL_SURFACE('',#4534,0.01);
#210=CYLINDRICAL_SURFACE('',#4536,0.038727);
#211=CYLINDRICAL_SURFACE('',#4539,0.0294270007);
#212=CYLINDRICAL_SURFACE('',#4544,0.038727);
#213=CYLINDRICAL_SURFACE('',#4548,0.03442700038);
#214=CYLINDRICAL_SURFACE('',#4552,0.038727);
#215=CYLINDRICAL_SURFACE('',#4556,0.03442700038);
#216=CYLINDRICAL_SURFACE('',#4560,0.038727);
#217=CYLINDRICAL_SURFACE('',#4564,0.03442700038);
#218=CYLINDRICAL_SURFACE('',#4568,0.038727);
#219=CYLINDRICAL_SURFACE('',#4572,0.0344270003800001);
#220=CYLINDRICAL_SURFACE('',#4577,0.014);
#221=CYLINDRICAL_SURFACE('',#4580,0.014);
#222=CYLINDRICAL_SURFACE('',#4584,0.01);
#223=CYLINDRICAL_SURFACE('',#4594,0.0075);
#224=CYLINDRICAL_SURFACE('',#4595,0.01);
#225=CYLINDRICAL_SURFACE('',#4597,0.031);
#226=CYLINDRICAL_SURFACE('',#4604,0.001);
#227=CYLINDRICAL_SURFACE('',#4606,0.001);
#228=CYLINDRICAL_SURFACE('',#4608,0.001);
#229=CYLINDRICAL_SURFACE('',#4610,0.001);
#230=CYLINDRICAL_SURFACE('',#4612,0.001);
#231=CYLINDRICAL_SURFACE('',#4614,0.001);
#232=CYLINDRICAL_SURFACE('',#4623,0.026);
#233=CYLINDRICAL_SURFACE('',#4630,0.026);
#234=CYLINDRICAL_SURFACE('',#4631,0.024);
#235=CYLINDRICAL_SURFACE('',#4632,0.001);
#236=CYLINDRICAL_SURFACE('',#4634,0.001);
#237=CYLINDRICAL_SURFACE('',#4641,0.0045);
#238=CYLINDRICAL_SURFACE('',#4645,0.0045);
#239=CYLINDRICAL_SURFACE('',#4663,0.024);
#240=CYLINDRICAL_SURFACE('',#4666,0.0045);
#241=CYLINDRICAL_SURFACE('',#4668,0.0045);
#242=CYLINDRICAL_SURFACE('',#4670,0.026);
#243=CYLINDRICAL_SURFACE('',#4674,0.026);
#244=CYLINDRICAL_SURFACE('',#4678,0.001);
#245=CYLINDRICAL_SURFACE('',#4681,0.001);
#246=CYLINDRICAL_SURFACE('',#4684,0.001);
#247=CYLINDRICAL_SURFACE('',#4687,0.001);
#248=CYLINDRICAL_SURFACE('',#4713,0.0655016995023668);
#249=CYLINDRICAL_SURFACE('',#4718,0.0655016995023668);
#250=CYLINDRICAL_SURFACE('',#4744,0.0325028673605553);
#251=CYLINDRICAL_SURFACE('',#4749,0.0151998);
#252=CYLINDRICAL_SURFACE('',#4752,0.0325028673605553);
#253=CYLINDRICAL_SURFACE('',#4759,0.011);
#254=CYLINDRICAL_SURFACE('',#4763,0.008207892);
#255=CYLINDRICAL_SURFACE('',#4768,0.0114910488);
#256=CYLINDRICAL_SURFACE('',#4776,0.0114910488);
#257=CYLINDRICAL_SURFACE('',#4781,0.008207892);
#258=CYLINDRICAL_SURFACE('',#4790,0.01);
#259=CYLINDRICAL_SURFACE('',#4795,0.01);
#260=CYLINDRICAL_SURFACE('',#4803,0.001);
#261=CYLINDRICAL_SURFACE('',#4804,0.001);
#262=CYLINDRICAL_SURFACE('',#4814,0.001);
#263=CYLINDRICAL_SURFACE('',#4819,0.001);
#264=CYLINDRICAL_SURFACE('',#4820,0.000999979135152545);
#265=CYLINDRICAL_SURFACE('',#4830,0.001);
#266=CYLINDRICAL_SURFACE('',#4842,0.001);
#267=CYLINDRICAL_SURFACE('',#4849,0.001);
#268=CYLINDRICAL_SURFACE('',#4854,0.001);
#269=CYLINDRICAL_SURFACE('',#4865,0.001);
#270=CYLINDRICAL_SURFACE('',#4877,0.001);
#271=CYLINDRICAL_SURFACE('',#4883,0.001);
#272=CYLINDRICAL_SURFACE('',#4884,0.001);
#273=CYLINDRICAL_SURFACE('',#4893,0.001);
#274=CYLINDRICAL_SURFACE('',#4898,0.001);
#275=CYLINDRICAL_SURFACE('',#4919,0.001);
#276=CYLINDRICAL_SURFACE('',#4936,0.001);
#277=CYLINDRICAL_SURFACE('',#4942,0.023);
#278=CYLINDRICAL_SURFACE('',#4945,0.024);
#279=CYLINDRICAL_SURFACE('',#4952,0.01);
#280=CYLINDRICAL_SURFACE('',#4955,0.011);
#281=CYLINDRICAL_SURFACE('',#4961,0.023455);
#282=CYLINDRICAL_SURFACE('',#4968,0.023455);
#283=CYLINDRICAL_SURFACE('',#4975,0.025);
#284=CYLINDRICAL_SURFACE('',#4979,0.023);
#285=CYLINDRICAL_SURFACE('',#4982,0.024);
#286=CYLINDRICAL_SURFACE('',#4987,0.005);
#287=CYLINDRICAL_SURFACE('',#4990,0.005);
#288=CYLINDRICAL_SURFACE('',#4991,0.003);
#289=CYLINDRICAL_SURFACE('',#4994,0.003);
#290=CYLINDRICAL_SURFACE('',#4996,0.04);
#291=CYLINDRICAL_SURFACE('',#4997,0.031);
#292=CYLINDRICAL_SURFACE('',#4999,0.029);
#293=CYLINDRICAL_SURFACE('',#5006,0.003);
#294=CYLINDRICAL_SURFACE('',#5010,0.029);
#295=CYLINDRICAL_SURFACE('',#5014,0.003);
#296=CYLINDRICAL_SURFACE('',#5021,0.003);
#297=CYLINDRICAL_SURFACE('',#5022,0.003);
#298=CYLINDRICAL_SURFACE('',#5023,0.003);
#299=CYLINDRICAL_SURFACE('',#5025,0.003);
#300=CYLINDRICAL_SURFACE('',#5028,0.025);
#301=CYLINDRICAL_SURFACE('',#5032,0.031);
#302=CYLINDRICAL_SURFACE('',#5034,0.024);
#303=CYLINDRICAL_SURFACE('',#5039,0.005);
#304=CYLINDRICAL_SURFACE('',#5045,0.005);
#305=CYLINDRICAL_SURFACE('',#5046,0.04);
#306=CYLINDRICAL_SURFACE('',#5055,0.023);
#307=CYLINDRICAL_SURFACE('',#5057,0.024);
#308=CIRCLE('',#4492,0.0055245);
#309=CIRCLE('',#4494,0.0047625);
#310=CIRCLE('',#4495,0.0047625);
#311=CIRCLE('',#4497,0.0039032404234375);
#312=CIRCLE('',#4499,0.0087376);
#313=CIRCLE('',#4501,0.0087376);
#314=CIRCLE('',#4503,0.0087376);
#315=CIRCLE('',#4505,0.0087376);
#316=CIRCLE('',#4507,0.0087376);
#317=CIRCLE('',#4509,0.0087376);
#318=CIRCLE('',#4515,0.041);
#319=CIRCLE('',#4516,0.039);
#320=CIRCLE('',#4518,0.041);
#321=CIRCLE('',#4519,0.039);
#322=CIRCLE('',#4524,0.039);
#323=CIRCLE('',#4525,0.039);
#324=CIRCLE('',#4528,0.0355);
#325=CIRCLE('',#4529,0.0355);
#326=CIRCLE('',#4535,0.01);
#327=CIRCLE('',#4537,0.038727);
#328=CIRCLE('',#4538,0.038727);
#329=CIRCLE('',#4540,0.0294270007);
#330=CIRCLE('',#4541,0.0294270007);
#331=CIRCLE('',#4543,0.038727);
#332=CIRCLE('',#4545,0.038727);
#333=CIRCLE('',#4547,0.03442700038);
#334=CIRCLE('',#4549,0.03442700038);
#335=CIRCLE('',#4551,0.038727);
#336=CIRCLE('',#4553,0.038727);
#337=CIRCLE('',#4555,0.03442700038);
#338=CIRCLE('',#4557,0.03442700038);
#339=CIRCLE('',#4559,0.038727);
#340=CIRCLE('',#4561,0.038727);
#341=CIRCLE('',#4563,0.03442700038);
#342=CIRCLE('',#4565,0.03442700038);
#343=CIRCLE('',#4567,0.038727);
#344=CIRCLE('',#4569,0.038727);
#345=CIRCLE('',#4571,0.0344270003800001);
#346=CIRCLE('',#4573,0.0344270003800001);
#347=CIRCLE('',#4578,0.014);
#348=CIRCLE('',#4581,0.014);
#349=CIRCLE('',#4583,0.01);
#350=CIRCLE('',#4589,0.0075);
#351=CIRCLE('',#4590,0.01);
#352=CIRCLE('',#4592,0.0075);
#353=CIRCLE('',#4593,0.01);
#354=CIRCLE('',#4598,0.031);
#355=CIRCLE('',#4599,0.031);
#356=CIRCLE('',#4601,0.03);
#357=CIRCLE('',#4603,0.03);
#358=CIRCLE('',#4613,0.001);
#359=CIRCLE('',#4615,0.001);
#360=CIRCLE('',#4618,0.026);
#361=CIRCLE('',#4619,0.024);
#362=CIRCLE('',#4621,0.027);
#363=CIRCLE('',#4622,0.026);
#364=CIRCLE('',#4625,0.026);
#365=CIRCLE('',#4626,0.027);
#366=CIRCLE('',#4628,0.026);
#367=CIRCLE('',#4629,0.024);
#368=CIRCLE('',#4633,0.001);
#369=CIRCLE('',#4635,0.001);
#370=CIRCLE('',#4640,0.0045);
#371=CIRCLE('',#4642,0.0045);
#372=CIRCLE('',#4644,0.0045);
#373=CIRCLE('',#4646,0.0045);
#374=CIRCLE('',#4652,0.027);
#375=CIRCLE('',#4653,0.0335028673605553);
#376=CIRCLE('',#4654,0.030591099482527);
#377=CIRCLE('',#4655,0.0335028673605553);
#378=CIRCLE('',#4657,0.0335028673605553);
#379=CIRCLE('',#4658,0.030591099482527);
#380=CIRCLE('',#4659,0.0335028673605553);
#381=CIRCLE('',#4660,0.027);
#382=CIRCLE('',#4664,0.024);
#383=CIRCLE('',#4665,0.024);
#384=CIRCLE('',#4667,0.0045);
#385=CIRCLE('',#4669,0.0045);
#386=CIRCLE('',#4671,0.026);
#387=CIRCLE('',#4672,0.026);
#388=CIRCLE('',#4675,0.026);
#389=CIRCLE('',#4676,0.026);
#390=CIRCLE('',#4679,0.001);
#391=CIRCLE('',#4680,0.001);
#392=CIRCLE('',#4682,0.001);
#393=CIRCLE('',#4683,0.001);
#394=CIRCLE('',#4685,0.001);
#395=CIRCLE('',#4686,0.001);
#396=CIRCLE('',#4688,0.001);
#397=CIRCLE('',#4689,0.001);
#398=CIRCLE('',#4693,0.009207892);
#399=CIRCLE('',#4694,0.0232046666802154);
#400=CIRCLE('',#4695,0.0665016995023668);
#401=CIRCLE('',#4696,0.0335028673605553);
#402=CIRCLE('',#4697,0.0381475271495645);
#403=CIRCLE('',#4698,0.0124910488);
#404=CIRCLE('',#4700,0.009207892);
#405=CIRCLE('',#4701,0.0232046666802154);
#406=CIRCLE('',#4702,0.0665016995023668);
#407=CIRCLE('',#4703,0.0335028673605553);
#408=CIRCLE('',#4704,0.0381475271495645);
#409=CIRCLE('',#4705,0.0124910488);
#410=CIRCLE('',#4707,0.0665016995023668);
#411=CIRCLE('',#4708,0.0147142518944256);
#412=CIRCLE('',#4709,0.0147142518944256);
#413=CIRCLE('',#4710,0.0665016995023668);
#414=CIRCLE('',#4711,0.0141998);
#415=CIRCLE('',#4712,0.0132);
#416=CIRCLE('',#4714,0.0655016995023668);
#417=CIRCLE('',#4715,0.0655016995023668);
#418=CIRCLE('',#4716,0.0655016995023668);
#419=CIRCLE('',#4717,0.0655016995023668);
#420=CIRCLE('',#4719,0.0655016995023668);
#421=CIRCLE('',#4720,0.0655016995023668);
#422=CIRCLE('',#4721,0.0655016995023668);
#423=CIRCLE('',#4722,0.0655016995023668);
#424=CIRCLE('',#4724,0.0665016995023668);
#425=CIRCLE('',#4725,0.0147142518944256);
#426=CIRCLE('',#4726,0.0147142518944256);
#427=CIRCLE('',#4727,0.0665016995023668);
#428=CIRCLE('',#4728,0.0141998);
#429=CIRCLE('',#4729,0.0132);
#430=CIRCLE('',#4731,0.0124910488);
#431=CIRCLE('',#4732,0.0381475271495645);
#432=CIRCLE('',#4733,0.0335028673605553);
#433=CIRCLE('',#4734,0.0665016995023668);
#434=CIRCLE('',#4735,0.0232046666802154);
#435=CIRCLE('',#4736,0.009207892);
#436=CIRCLE('',#4738,0.0124910488);
#437=CIRCLE('',#4739,0.0381475271495645);
#438=CIRCLE('',#4740,0.0335028673605553);
#439=CIRCLE('',#4741,0.0665016995023668);
#440=CIRCLE('',#4742,0.0232046666802154);
#441=CIRCLE('',#4743,0.009207892);
#442=CIRCLE('',#4745,0.0325028673605553);
#443=CIRCLE('',#4746,0.0325028673605553);
#444=CIRCLE('',#4747,0.0325028673605553);
#445=CIRCLE('',#4748,0.0325028673605553);
#446=CIRCLE('',#4750,0.0151998);
#447=CIRCLE('',#4751,0.0151998);
#448=CIRCLE('',#4753,0.0325028673605553);
#449=CIRCLE('',#4754,0.0325028673605553);
#450=CIRCLE('',#4755,0.0325028673605553);
#451=CIRCLE('',#4756,0.0325028673605553);
#452=CIRCLE('',#4760,0.011);
#453=CIRCLE('',#4761,0.011);
#454=CIRCLE('',#4764,0.008207892);
#455=CIRCLE('',#4765,0.008207892);
#456=CIRCLE('',#4766,0.008207892);
#457=CIRCLE('',#4769,0.0114910488);
#458=CIRCLE('',#4770,0.0114910488);
#459=CIRCLE('',#4771,0.0114910488);
#460=CIRCLE('',#4773,0.007207892);
#461=CIRCLE('',#4774,0.0104910488);
#462=CIRCLE('',#4777,0.0114910488);
#463=CIRCLE('',#4778,0.0114910488);
#464=CIRCLE('',#4779,0.0114910488);
#465=CIRCLE('',#4782,0.008207892);
#466=CIRCLE('',#4783,0.008207892);
#467=CIRCLE('',#4784,0.008207892);
#468=CIRCLE('',#4786,0.0104910488);
#469=CIRCLE('',#4787,0.007207892);
#470=CIRCLE('',#4789,0.0154861077840428);
#471=CIRCLE('',#4792,0.0154861077840428);
#472=CIRCLE('',#4794,0.0154861077840428);
#473=CIRCLE('',#4797,0.0154861077840428);
#474=CIRCLE('',#4799,0.0312780474522577);
#475=CIRCLE('',#4801,0.0312780474522577);
#476=CIRCLE('',#4807,0.012);
#477=CIRCLE('',#4808,0.0122);
#478=CIRCLE('',#4810,0.012);
#479=CIRCLE('',#4811,0.0122);
#480=CIRCLE('',#4813,0.001);
#481=CIRCLE('',#4815,0.001);
#482=CIRCLE('',#4817,0.001);
#483=CIRCLE('',#4822,0.001);
#484=CIRCLE('',#4824,0.001);
#485=CIRCLE('',#4825,0.001);
#486=CIRCLE('',#4826,0.001);
#487=CIRCLE('',#4827,0.001);
#488=CIRCLE('',#4829,0.001);
#489=CIRCLE('',#4831,0.001);
#490=CIRCLE('',#4833,0.001);
#491=CIRCLE('',#4834,0.001);
#492=CIRCLE('',#4836,0.001);
#493=CIRCLE('',#4837,0.001);
#494=CIRCLE('',#4838,0.001);
#495=CIRCLE('',#4839,0.001);
#496=CIRCLE('',#4841,0.001);
#497=CIRCLE('',#4843,0.001);
#498=CIRCLE('',#4845,0.001);
#499=CIRCLE('',#4846,0.001);
#500=CIRCLE('',#4848,0.001);
#501=CIRCLE('',#4850,0.001);
#502=CIRCLE('',#4852,0.001);
#503=CIRCLE('',#4857,0.001);
#504=CIRCLE('',#4859,0.001);
#505=CIRCLE('',#4860,0.001);
#506=CIRCLE('',#4861,0.001);
#507=CIRCLE('',#4862,0.001);
#508=CIRCLE('',#4864,0.001);
#509=CIRCLE('',#4866,0.001);
#510=CIRCLE('',#4868,0.001);
#511=CIRCLE('',#4869,0.001);
#512=CIRCLE('',#4871,0.001);
#513=CIRCLE('',#4872,0.001);
#514=CIRCLE('',#4873,0.001);
#515=CIRCLE('',#4874,0.001);
#516=CIRCLE('',#4876,0.001);
#517=CIRCLE('',#4878,0.001);
#518=CIRCLE('',#4880,0.001);
#519=CIRCLE('',#4881,0.001);
#520=CIRCLE('',#4887,0.001);
#521=CIRCLE('',#4889,0.001);
#522=CIRCLE('',#4892,0.001);
#523=CIRCLE('',#4894,0.001);
#524=CIRCLE('',#4897,0.001);
#525=CIRCLE('',#4899,0.001);
#526=CIRCLE('',#4902,0.001);
#527=CIRCLE('',#4904,0.001);
#528=CIRCLE('',#4907,0.001);
#529=CIRCLE('',#4908,0.001);
#530=CIRCLE('',#4910,0.001);
#531=CIRCLE('',#4912,0.001);
#532=CIRCLE('',#4914,0.001);
#533=CIRCLE('',#4916,0.001);
#534=CIRCLE('',#4924,0.001);
#535=CIRCLE('',#4925,0.001);
#536=CIRCLE('',#4927,0.001);
#537=CIRCLE('',#4929,0.001);
#538=CIRCLE('',#4931,0.001);
#539=CIRCLE('',#4933,0.001);
#540=CIRCLE('',#4943,0.023);
#541=CIRCLE('',#4944,0.023);
#542=CIRCLE('',#4946,0.024);
#543=CIRCLE('',#4947,0.024);
#544=CIRCLE('',#4953,0.01);
#545=CIRCLE('',#4954,0.01);
#546=CIRCLE('',#4956,0.011);
#547=CIRCLE('',#4957,0.011);
#548=CIRCLE('',#4962,0.023455);
#549=CIRCLE('',#4963,0.023455);
#550=CIRCLE('',#4965,0.031);
#551=CIRCLE('',#4966,0.0316935480501236);
#552=CIRCLE('',#4967,0.031693548050133);
#553=CIRCLE('',#4969,0.023455);
#554=CIRCLE('',#4970,0.023455);
#555=CIRCLE('',#4972,0.025);
#556=CIRCLE('',#4980,0.023);
#557=CIRCLE('',#4981,0.023);
#558=CIRCLE('',#4984,0.00499999999999991);
#559=CIRCLE('',#4985,0.04);
#560=CIRCLE('',#4986,0.005);
#561=CIRCLE('',#4998,0.031);
#562=CIRCLE('',#5000,0.029);
#563=CIRCLE('',#5001,0.029);
#564=CIRCLE('',#5002,0.00298497776938405);
#565=CIRCLE('',#5003,0.00298497542639763);
#566=CIRCLE('',#5004,0.00298498584851454);
#567=CIRCLE('',#5005,0.00298498508188116);
#568=CIRCLE('',#5011,0.029);
#569=CIRCLE('',#5012,0.029);
#570=CIRCLE('',#5013,0.00298508178884043);
#571=CIRCLE('',#5018,0.025);
#572=CIRCLE('',#5020,0.031);
#573=CIRCLE('',#5033,0.031);
#574=CIRCLE('',#5036,0.00499999999999984);
#575=CIRCLE('',#5037,0.04);
#576=CIRCLE('',#5038,0.0049999999999997);
#577=CIRCLE('',#5041,0.0316935480501328);
#578=CIRCLE('',#5043,0.0316935480501328);
#579=CIRCLE('',#5053,0.024);
#580=CIRCLE('',#5054,0.023);
#581=CIRCLE('',#5056,0.023);
#582=CIRCLE('',#5058,0.024);
#583=B_SPLINE_CURVE_WITH_KNOTS('',3,(#6407,#6408,#6409,#6410),
 .UNSPECIFIED.,.F.,.F.,(4,4),(2.38073112704607E-7,0.00510460360858836),
 .UNSPECIFIED.);
#584=B_SPLINE_CURVE_WITH_KNOTS('',3,(#6412,#6413,#6414,#6415),
 .UNSPECIFIED.,.F.,.F.,(4,4),(0.00510460360858836,0.0101898849784681),
 .UNSPECIFIED.);
#585=B_SPLINE_CURVE_WITH_KNOTS('',3,(#6424,#6425,#6426,#6427),
 .UNSPECIFIED.,.F.,.F.,(4,4),(2.38073112713057E-7,0.00510460360858837),
 .UNSPECIFIED.);
#586=B_SPLINE_CURVE_WITH_KNOTS('',3,(#6429,#6430,#6431,#6432),
 .UNSPECIFIED.,.F.,.F.,(4,4),(0.00510460360858837,0.0101898849784681),
 .UNSPECIFIED.);
#587=B_SPLINE_CURVE_WITH_KNOTS('',3,(#6438,#6439,#6440,#6441),
 .UNSPECIFIED.,.F.,.F.,(4,4),(0.0141037246460291,0.0192101526638855),
 .UNSPECIFIED.);
#588=B_SPLINE_CURVE_WITH_KNOTS('',3,(#6443,#6444,#6445,#6446),
 .UNSPECIFIED.,.F.,.F.,(4,4),(0.00900032873565963,0.0141037246460291),
 .UNSPECIFIED.);
#589=B_SPLINE_CURVE_WITH_KNOTS('',3,(#6452,#6453,#6454,#6455),
 .UNSPECIFIED.,.F.,.F.,(4,4),(2.38073112724182E-7,0.00510460360858838),
 .UNSPECIFIED.);
#590=B_SPLINE_CURVE_WITH_KNOTS('',3,(#6457,#6458,#6459,#6460),
 .UNSPECIFIED.,.F.,.F.,(4,4),(0.00510460360858838,0.0101898849784681),
 .UNSPECIFIED.);
#591=B_SPLINE_CURVE_WITH_KNOTS('',3,(#6466,#6467,#6468,#6469),
 .UNSPECIFIED.,.F.,.F.,(4,4),(2.38073112713057E-7,0.00510460360858837),
 .UNSPECIFIED.);
#592=B_SPLINE_CURVE_WITH_KNOTS('',3,(#6471,#6472,#6473,#6474),
 .UNSPECIFIED.,.F.,.F.,(4,4),(0.00510460360858837,0.0101898849784681),
 .UNSPECIFIED.);
#593=B_SPLINE_CURVE_WITH_KNOTS('',3,(#6477,#6478,#6479,#6480),
 .UNSPECIFIED.,.F.,.F.,(4,4),(0.00900032873565963,0.0141037246460291),
 .UNSPECIFIED.);
#594=B_SPLINE_CURVE_WITH_KNOTS('',3,(#6482,#6483,#6484,#6485),
 .UNSPECIFIED.,.F.,.F.,(4,4),(0.0141037246460291,0.0192101526638855),
 .UNSPECIFIED.);
#595=B_SPLINE_CURVE_WITH_KNOTS('',3,(#6555,#6556,#6557,#6558,#6559,#6560,
#6561,#6562,#6563,#6564,#6565,#6566,#6567,#6568,#6569,#6570,#6571,#6572,
#6573),.UNSPECIFIED.,.T.,.F.,(1,1,1,1,1,1,1,1,1,1,1,1,1,1,1,1,1,1,1,1,1,
1,1),(-0.0118110140186832,-0.00787400934578877,-0.00393700467289439,0.,
0.00393700467289439,0.00787400934578878,0.0118110140186832,0.0157480186915776,
0.0196850233644719,0.0236220280373663,0.0275590327102607,0.0314960373831551,
0.0354330420560495,0.0393700467289439,0.0433070514018383,0.0472440560747327,
0.0511810607476271,0.0551180654205214,0.0590550700934158,0.0629920747663102,
0.0669290794392046,0.070866084112099,0.0748030887849934),.UNSPECIFIED.);
#596=B_SPLINE_CURVE_WITH_KNOTS('',3,(#6578,#6579,#6580,#6581,#6582,#6583,
#6584,#6585,#6586,#6587,#6588,#6589,#6590,#6591,#6592,#6593,#6594,#6595,
#6596,#6597,#6598),.UNSPECIFIED.,.T.,.F.,(1,1,1,1,1,1,1,1,1,1,1,1,1,1,1,
1,1,1,1,1,1,1,1,1,1),(-0.0165527839474341,-0.0110351892982894,-0.00551759464914471,
0.,0.00551759464914471,0.0110351892982894,0.0165527839474341,0.0220703785965788,
0.0275879732457236,0.0331055678948683,0.038623162544013,0.0441407571931577,
0.0496583518423024,0.0551759464914471,0.0579347438160195,0.0606935411405918,
0.0634523384651642,0.0662111357897365,0.0717287304388812,0.077246325088026,
0.0827639197371707,0.0882815143863154,0.0937991090354601,0.0993167036846048,
0.10483429833375),.UNSPECIFIED.);
#597=B_SPLINE_CURVE_WITH_KNOTS('',3,(#6604,#6605,#6606,#6607,#6608,#6609,
#6610,#6611,#6612,#6613,#6614,#6615,#6616,#6617,#6618,#6619,#6620,#6621,
#6622,#6623,#6624),.UNSPECIFIED.,.T.,.F.,(1,1,1,1,1,1,1,1,1,1,1,1,1,1,1,
1,1,1,1,1,1,1,1,1,1),(-0.0165527839474341,-0.0110351892982894,-0.00551759464914471,
0.,0.00551759464914471,0.0110351892982894,0.0165527839474341,0.0220703785965788,
0.0275879732457236,0.0331055678948683,0.038623162544013,0.0441407571931577,
0.0496583518423024,0.0551759464914471,0.0579347438160195,0.0606935411405918,
0.0634523384651642,0.0662111357897365,0.0717287304388812,0.077246325088026,
0.0827639197371707,0.0882815143863154,0.0937991090354601,0.0993167036846048,
0.10483429833375),.UNSPECIFIED.);
#598=B_SPLINE_CURVE_WITH_KNOTS('',3,(#6629,#6630,#6631,#6632,#6633,#6634,
#6635,#6636,#6637,#6638,#6639,#6640,#6641,#6642,#6643,#6644,#6645,#6646,
#6647),.UNSPECIFIED.,.T.,.F.,(1,1,1,1,1,1,1,1,1,1,1,1,1,1,1,1,1,1,1,1,1,
1,1),(-0.0118110140186832,-0.00787400934578878,-0.00393700467289439,0.,
0.00393700467289439,0.00787400934578878,0.0118110140186832,0.0157480186915776,
0.019685023364472,0.0236220280373663,0.0275590327102607,0.0314960373831551,
0.0354330420560495,0.0393700467289439,0.0433070514018383,0.0472440560747327,
0.0511810607476271,0.0551180654205215,0.0590550700934159,0.0629920747663102,
0.0669290794392046,0.070866084112099,0.0748030887849934),.UNSPECIFIED.);
#599=B_SPLINE_CURVE_WITH_KNOTS('',3,(#6739,#6740,#6741,#6742,#6743),
 .UNSPECIFIED.,.F.,.F.,(4,1,4),(0.,0.000805913704203702,0.0016118274084074),
 .UNSPECIFIED.);
#600=B_SPLINE_CURVE_WITH_KNOTS('',3,(#6747,#6748,#6749,#6750,#6751),
 .UNSPECIFIED.,.F.,.F.,(4,1,4),(0.,0.000805913704203702,0.0016118274084074),
 .UNSPECIFIED.);
#601=B_SPLINE_CURVE_WITH_KNOTS('',3,(#6753,#6754,#6755,#6756,#6757),
 .UNSPECIFIED.,.F.,.F.,(4,1,4),(0.,0.000805913704203699,0.0016118274084074),
 .UNSPECIFIED.);
#602=B_SPLINE_CURVE_WITH_KNOTS('',3,(#6759,#6760,#6761,#6762,#6763),
 .UNSPECIFIED.,.F.,.F.,(4,1,4),(0.,0.000805913704203701,0.0016118274084074),
 .UNSPECIFIED.);
#603=B_SPLINE_CURVE_WITH_KNOTS('',3,(#6818,#6819,#6820,#6821,#6822),
 .UNSPECIFIED.,.F.,.F.,(4,1,4),(0.000383476419715099,0.0011765940099438,
0.0019697116001725),.UNSPECIFIED.);
#604=B_SPLINE_CURVE_WITH_KNOTS('',3,(#6826,#6827,#6828,#6829,#6830),
 .UNSPECIFIED.,.F.,.F.,(4,1,4),(0.00616146542423319,0.00695359511819705,
0.0077457248121609),.UNSPECIFIED.);
#605=B_SPLINE_CURVE_WITH_KNOTS('',3,(#6838,#6839,#6840,#6841,#6842),
 .UNSPECIFIED.,.F.,.F.,(4,1,4),(0.00437149970837484,0.00516403730127254,
0.00595657489417023),.UNSPECIFIED.);
#606=B_SPLINE_CURVE_WITH_KNOTS('',3,(#6846,#6847,#6848,#6849,#6850),
 .UNSPECIFIED.,.F.,.F.,(4,1,4),(0.00493537550573997,0.00572807532890887,
0.00652077515207777),.UNSPECIFIED.);
#607=B_SPLINE_CURVE_WITH_KNOTS('',3,(#6965,#6966,#6967,#6968,#6969,#6970,
#6971,#6972,#6973,#6974,#6975,#6976,#6977,#6978,#6979,#6980,#6981,#6982,
#6983),.UNSPECIFIED.,.T.,.F.,(1,1,1,1,1,1,1,1,1,1,1,1,1,1,1,1,1,1,1,1,1,
1,1),(-0.00575205114744636,-0.00383470076496424,-0.00191735038248212,0.,
0.00191735038248212,0.00383470076496424,0.00575205114744636,0.00766940152992848,
0.0095867519124106,0.0115041022948927,0.0134214526773748,0.015338803059857,
0.0172561534423391,0.0191735038248212,0.0210908542073033,0.0230082045897854,
0.0249255549722676,0.0268429053547497,0.0287602557372318,0.0306776061197139,
0.032594956502196,0.0345123068846782,0.0364296572671603),.UNSPECIFIED.);
#608=B_SPLINE_CURVE_WITH_KNOTS('',3,(#6988,#6989,#6990,#6991,#6992,#6993,
#6994,#6995,#6996,#6997,#6998,#6999,#7000,#7001,#7002,#7003,#7004,#7005,
#7006),.UNSPECIFIED.,.T.,.F.,(1,1,1,1,1,1,1,1,1,1,1,1,1,1,1,1,1,1,1,1,1,
1,1),(-0.00575205114744637,-0.00383470076496424,-0.00191735038248212,0.,
0.00191735038248212,0.00383470076496425,0.00575205114744637,0.00766940152992849,
0.00958675191241062,0.0115041022948927,0.0134214526773749,0.015338803059857,
0.0172561534423391,0.0191735038248212,0.0210908542073034,0.0230082045897855,
0.0249255549722676,0.0268429053547497,0.0287602557372319,0.030677606119714,
0.0325949565021961,0.0345123068846782,0.0364296572671603),.UNSPECIFIED.);
#609=B_SPLINE_CURVE_WITH_KNOTS('',3,(#7047,#7048,#7049,#7050,#7051),
 .UNSPECIFIED.,.F.,.F.,(4,1,4),(0.00437149970837484,0.00516403730127254,
0.00595657489417023),.UNSPECIFIED.);
#610=B_SPLINE_CURVE_WITH_KNOTS('',3,(#7052,#7053,#7054,#7055,#7056),
 .UNSPECIFIED.,.F.,.F.,(4,1,4),(0.00493537550573997,0.00572807532890887,
0.00652077515207777),.UNSPECIFIED.);
#611=B_SPLINE_CURVE_WITH_KNOTS('',3,(#7058,#7059,#7060,#7061,#7062),
 .UNSPECIFIED.,.F.,.F.,(4,1,4),(0.000383476419715099,0.00117659400994475,
0.00196971160017441),.UNSPECIFIED.);
#612=B_SPLINE_CURVE_WITH_KNOTS('',3,(#7063,#7064,#7065,#7066,#7067),
 .UNSPECIFIED.,.F.,.F.,(4,1,4),(0.00616146542423319,0.00695359511819705,
0.0077457248121609),.UNSPECIFIED.);
#613=B_SPLINE_CURVE_WITH_KNOTS('',3,(#7123,#7124,#7125,#7126,#7127,#7128,
#7129),.UNSPECIFIED.,.F.,.F.,(4,1,1,1,4),(0.00352549128828216,0.00696797821694395,
0.0104104651456057,0.0138529520742675,0.0172954390029293),.UNSPECIFIED.);
#614=B_SPLINE_CURVE_WITH_KNOTS('',3,(#7137,#7138,#7139,#7140,#7141,#7142,
#7143),.UNSPECIFIED.,.F.,.F.,(4,1,1,1,4),(0.,0.00340629880233305,0.0068125976046661,
0.0102188964069992,0.0136251952093322),.UNSPECIFIED.);
#615=B_SPLINE_CURVE_WITH_KNOTS('',3,(#7147,#7148,#7149,#7150,#7151,#7152,
#7153),.UNSPECIFIED.,.F.,.F.,(4,1,1,1,4),(0.,0.00340629880233381,0.00681259760466761,
0.0102188964070014,0.0136251952093352),.UNSPECIFIED.);
#616=B_SPLINE_CURVE_WITH_KNOTS('',3,(#7162,#7163,#7164,#7165,#7166,#7167,
#7168),.UNSPECIFIED.,.F.,.F.,(4,1,1,1,4),(0.00352549128828207,0.00696797821694389,
0.0104104651456057,0.0138529520742675,0.0172954390029293),.UNSPECIFIED.);
#617=B_SPLINE_CURVE_WITH_KNOTS('',3,(#7232,#7233,#7234,#7235,#7236),
 .UNSPECIFIED.,.F.,.F.,(4,1,4),(0.,0.0064793361194087,0.0129586722388174),
 .UNSPECIFIED.);
#618=B_SPLINE_CURVE_WITH_KNOTS('',3,(#7244,#7245,#7246,#7247,#7248),
 .UNSPECIFIED.,.F.,.F.,(4,1,4),(0.,0.00645902084593716,0.0129180416918743),
 .UNSPECIFIED.);
#619=B_SPLINE_CURVE_WITH_KNOTS('',3,(#7260,#7261,#7262,#7263,#7264),
 .UNSPECIFIED.,.F.,.F.,(4,1,4),(0.,0.00647933611940867,0.0129586722388173),
 .UNSPECIFIED.);
#620=B_SPLINE_CURVE_WITH_KNOTS('',3,(#7272,#7273,#7274,#7275,#7276),
 .UNSPECIFIED.,.F.,.F.,(4,1,4),(0.,0.00645902084593563,0.0129180416918713),
 .UNSPECIFIED.);
#621=B_SPLINE_CURVE_WITH_KNOTS('',3,(#7298,#7299,#7300,#7301),
 .UNSPECIFIED.,.F.,.F.,(4,4),(8.13151629364128E-20,0.00716108843954949),
 .UNSPECIFIED.);
#622=B_SPLINE_CURVE_WITH_KNOTS('',3,(#7311,#7312,#7313,#7314),
 .UNSPECIFIED.,.F.,.F.,(4,4),(0.,0.00710594861592948),.UNSPECIFIED.);
#623=B_SPLINE_CURVE_WITH_KNOTS('',3,(#7316,#7317,#7318,#7319),
 .UNSPECIFIED.,.F.,.F.,(4,4),(0.,1.),.UNSPECIFIED.);
#624=B_SPLINE_CURVE_WITH_KNOTS('',3,(#7329,#7330,#7331,#7332),
 .UNSPECIFIED.,.F.,.F.,(4,4),(0.,0.00411946769479083),.UNSPECIFIED.);
#625=B_SPLINE_CURVE_WITH_KNOTS('',3,(#7360,#7361,#7362,#7363),
 .UNSPECIFIED.,.F.,.F.,(4,4),(0.,0.00411946769479048),.UNSPECIFIED.);
#626=B_SPLINE_CURVE_WITH_KNOTS('',3,(#7374,#7375,#7376,#7377),
 .UNSPECIFIED.,.F.,.F.,(4,4),(1.35525271560688E-20,0.00716108843954742),
 .UNSPECIFIED.);
#627=B_SPLINE_CURVE_WITH_KNOTS('',3,(#7384,#7385,#7386,#7387),
 .UNSPECIFIED.,.F.,.F.,(4,4),(0.,0.00710594861592814),.UNSPECIFIED.);
#628=B_SPLINE_CURVE_WITH_KNOTS('',3,(#7389,#7390,#7391,#7392),
 .UNSPECIFIED.,.F.,.F.,(4,4),(0.,1.),.UNSPECIFIED.);
#629=B_SPLINE_CURVE_WITH_KNOTS('',3,(#7403,#7404,#7405,#7406),
 .UNSPECIFIED.,.F.,.F.,(4,4),(0.000458247724612459,0.00515055882881692),
 .UNSPECIFIED.);
#630=B_SPLINE_CURVE_WITH_KNOTS('',3,(#7411,#7412,#7413,#7414,#7415,#7416),
 .UNSPECIFIED.,.F.,.F.,(4,1,1,4),(0.00143499903345957,0.00481436180627339,
0.00819372457908721,0.0149524501247149),.UNSPECIFIED.);
#631=B_SPLINE_CURVE_WITH_KNOTS('',3,(#7417,#7418,#7419,#7420,#7421),
 .UNSPECIFIED.,.F.,.F.,(4,1,4),(0.,0.00387944920372668,0.00775889840745336),
 .UNSPECIFIED.);
#632=B_SPLINE_CURVE_WITH_KNOTS('',3,(#7423,#7424,#7425,#7426),
 .UNSPECIFIED.,.F.,.F.,(4,4),(0.000458247724612459,0.00515055882881692),
 .UNSPECIFIED.);
#633=B_SPLINE_CURVE_WITH_KNOTS('',3,(#7430,#7431,#7432,#7433),
 .UNSPECIFIED.,.F.,.F.,(4,4),(0.,1.),.UNSPECIFIED.);
#634=B_SPLINE_CURVE_WITH_KNOTS('',3,(#7435,#7436,#7437,#7438,#7439,#7440),
 .UNSPECIFIED.,.F.,.F.,(4,1,1,4),(0.,0.00671446169703845,0.0100716925455577,
0.0134289233940769),.UNSPECIFIED.);
#635=B_SPLINE_CURVE_WITH_KNOTS('',3,(#7443,#7444,#7445,#7446,#7447),
 .UNSPECIFIED.,.F.,.F.,(4,1,4),(0.,0.00391314275686453,0.00782628551372907),
 .UNSPECIFIED.);
#636=B_SPLINE_CURVE_WITH_KNOTS('',3,(#7449,#7450,#7451,#7452),
 .UNSPECIFIED.,.F.,.F.,(4,4),(0.000458247724612439,0.00515055882881691),
 .UNSPECIFIED.);
#637=B_SPLINE_CURVE_WITH_KNOTS('',3,(#7457,#7458,#7459,#7460,#7461,#7462),
 .UNSPECIFIED.,.F.,.F.,(4,1,1,4),(0.00143499903345957,0.00481436180627316,
0.00819372457908675,0.0149524501247139),.UNSPECIFIED.);
#638=B_SPLINE_CURVE_WITH_KNOTS('',3,(#7463,#7464,#7465,#7466,#7467),
 .UNSPECIFIED.,.F.,.F.,(4,1,4),(0.,0.00387944920372737,0.00775889840745473),
 .UNSPECIFIED.);
#639=B_SPLINE_CURVE_WITH_KNOTS('',3,(#7469,#7470,#7471,#7472),
 .UNSPECIFIED.,.F.,.F.,(4,4),(0.000458247724612439,0.00515055882881689),
 .UNSPECIFIED.);
#640=B_SPLINE_CURVE_WITH_KNOTS('',3,(#7476,#7477,#7478,#7479),
 .UNSPECIFIED.,.F.,.F.,(4,4),(0.,1.),.UNSPECIFIED.);
#641=B_SPLINE_CURVE_WITH_KNOTS('',3,(#7481,#7482,#7483,#7484,#7485,#7486),
 .UNSPECIFIED.,.F.,.F.,(4,1,1,4),(0.,0.00671446169703849,0.0100716925455577,
0.013428923394077),.UNSPECIFIED.);
#642=B_SPLINE_CURVE_WITH_KNOTS('',3,(#7489,#7490,#7491,#7492,#7493),
 .UNSPECIFIED.,.F.,.F.,(4,1,4),(0.,0.00391314275686577,0.00782628551373154),
 .UNSPECIFIED.);
#643=B_SPLINE_CURVE_WITH_KNOTS('',3,(#7495,#7496,#7497,#7498,#7499),
 .UNSPECIFIED.,.F.,.F.,(4,1,4),(0.,0.00647222827986434,0.0129444565597287),
 .UNSPECIFIED.);
#644=B_SPLINE_CURVE_WITH_KNOTS('',3,(#7503,#7504,#7505,#7506,#7507),
 .UNSPECIFIED.,.F.,.F.,(4,1,4),(0.00137904255227218,0.00786045945981697,
0.0143418763673618),.UNSPECIFIED.);
#645=B_SPLINE_CURVE_WITH_KNOTS('',3,(#7508,#7509,#7510,#7511),
 .UNSPECIFIED.,.F.,.F.,(4,4),(0.,0.00447796131591151),.UNSPECIFIED.);
#646=B_SPLINE_CURVE_WITH_KNOTS('',3,(#7513,#7514,#7515,#7516,#7517),
 .UNSPECIFIED.,.F.,.F.,(4,1,4),(0.,0.00647222827986436,0.0129444565597287),
 .UNSPECIFIED.);
#647=B_SPLINE_CURVE_WITH_KNOTS('',3,(#7521,#7522,#7523,#7524,#7525),
 .UNSPECIFIED.,.F.,.F.,(4,1,4),(0.00137904255227228,0.00786045945981642,
0.0143418763673606),.UNSPECIFIED.);
#648=B_SPLINE_CURVE_WITH_KNOTS('',3,(#7526,#7527,#7528,#7529),
 .UNSPECIFIED.,.F.,.F.,(4,4),(0.,0.00447796131591189),.UNSPECIFIED.);
#649=B_SPLINE_CURVE_WITH_KNOTS('',3,(#7531,#7532,#7533,#7534,#7535),
 .UNSPECIFIED.,.F.,.F.,(4,1,4),(0.,0.000781285135510639,0.00156257027102128),
 .UNSPECIFIED.);
#650=B_SPLINE_CURVE_WITH_KNOTS('',3,(#7536,#7537,#7538,#7539,#7540),
 .UNSPECIFIED.,.F.,.F.,(4,1,4),(0.,0.000781285135510629,0.00156257027102126),
 .UNSPECIFIED.);
#651=B_SPLINE_CURVE_WITH_KNOTS('',3,(#7542,#7543,#7544,#7545,#7546),
 .UNSPECIFIED.,.F.,.F.,(4,1,4),(0.,0.000781288146365363,0.00156257629273073),
 .UNSPECIFIED.);
#652=B_SPLINE_CURVE_WITH_KNOTS('',3,(#7548,#7549,#7550,#7551,#7552),
 .UNSPECIFIED.,.F.,.F.,(4,1,4),(0.,0.000781288146365363,0.00156257629273073),
 .UNSPECIFIED.);
#653=B_SPLINE_CURVE_WITH_KNOTS('',3,(#7566,#7567,#7568,#7569,#7570),
 .UNSPECIFIED.,.F.,.F.,(4,1,4),(0.,0.000781272382823816,0.00156254476564763),
 .UNSPECIFIED.);
#654=B_SPLINE_CURVE_WITH_KNOTS('',3,(#7572,#7573,#7574,#7575,#7576),
 .UNSPECIFIED.,.F.,.F.,(4,1,4),(0.,0.000781270211991802,0.0015625404239836),
 .UNSPECIFIED.);
#655=B_SPLINE_CURVE_WITH_KNOTS('',3,(#7593,#7594,#7595,#7596,#7597),
 .UNSPECIFIED.,.F.,.F.,(4,1,4),(0.,0.000781272382824027,0.00156254476564805),
 .UNSPECIFIED.);
#656=B_SPLINE_CURVE_WITH_KNOTS('',3,(#7616,#7617,#7618,#7619,#7620),
 .UNSPECIFIED.,.F.,.F.,(4,1,4),(0.,0.5,1.),.UNSPECIFIED.);
#657=B_SPLINE_CURVE_WITH_KNOTS('',3,(#7622,#7623,#7624,#7625,#7626),
 .UNSPECIFIED.,.F.,.F.,(4,1,4),(0.,0.000781270211991983,0.00156254042398397),
 .UNSPECIFIED.);
#658=B_SPLINE_CURVE_WITH_KNOTS('',3,(#7628,#7629,#7630,#7631,#7632),
 .UNSPECIFIED.,.F.,.F.,(4,1,4),(0.,0.5,1.),.UNSPECIFIED.);
#659=B_SPLINE_CURVE_WITH_KNOTS('',3,(#7751,#7752,#7753,#7754,#7755),
 .UNSPECIFIED.,.F.,.F.,(4,1,4),(0.,0.000781272382823819,0.00156254476564764),
 .UNSPECIFIED.);
#660=B_SPLINE_CURVE_WITH_KNOTS('',3,(#7757,#7758,#7759,#7760,#7761),
 .UNSPECIFIED.,.F.,.F.,(4,1,4),(0.,0.000781270211991816,0.00156254042398363),
 .UNSPECIFIED.);
#661=B_SPLINE_CURVE_WITH_KNOTS('',3,(#7778,#7779,#7780,#7781,#7782),
 .UNSPECIFIED.,.F.,.F.,(4,1,4),(0.,0.000781272382824017,0.00156254476564803),
 .UNSPECIFIED.);
#662=B_SPLINE_CURVE_WITH_KNOTS('',3,(#7801,#7802,#7803,#7804,#7805),
 .UNSPECIFIED.,.F.,.F.,(4,1,4),(0.,0.5,1.),.UNSPECIFIED.);
#663=B_SPLINE_CURVE_WITH_KNOTS('',3,(#7807,#7808,#7809,#7810,#7811),
 .UNSPECIFIED.,.F.,.F.,(4,1,4),(0.,0.000781270211991975,0.00156254042398395),
 .UNSPECIFIED.);
#664=B_SPLINE_CURVE_WITH_KNOTS('',3,(#7813,#7814,#7815,#7816,#7817),
 .UNSPECIFIED.,.F.,.F.,(4,1,4),(0.,0.5,1.),.UNSPECIFIED.);
#665=B_SPLINE_CURVE_WITH_KNOTS('',3,(#7935,#7936,#7937,#7938,#7939),
 .UNSPECIFIED.,.F.,.F.,(4,1,4),(0.,0.000781288146365333,0.00156257629273067),
 .UNSPECIFIED.);
#666=B_SPLINE_CURVE_WITH_KNOTS('',3,(#7940,#7941,#7942,#7943,#7944),
 .UNSPECIFIED.,.F.,.F.,(4,1,4),(0.,0.000781288146365363,0.00156257629273073),
 .UNSPECIFIED.);
#667=B_SPLINE_CURVE_WITH_KNOTS('',3,(#7946,#7947,#7948,#7949,#7950),
 .UNSPECIFIED.,.F.,.F.,(4,1,4),(0.,0.000781285135510639,0.00156257027102128),
 .UNSPECIFIED.);
#668=B_SPLINE_CURVE_WITH_KNOTS('',3,(#7952,#7953,#7954,#7955,#7956),
 .UNSPECIFIED.,.F.,.F.,(4,1,4),(0.,0.000781285135510639,0.00156257027102128),
 .UNSPECIFIED.);
#669=B_SPLINE_CURVE_WITH_KNOTS('',3,(#7990,#7991,#7992,#7993),
 .UNSPECIFIED.,.F.,.F.,(4,4),(1.11076830053021E-17,0.000876980038522517),
 .UNSPECIFIED.);
#670=B_SPLINE_CURVE_WITH_KNOTS('',3,(#7995,#7996,#7997,#7998),
 .UNSPECIFIED.,.F.,.F.,(4,4),(1.11076830053021E-17,0.000876980038522516),
 .UNSPECIFIED.);
#671=B_SPLINE_CURVE_WITH_KNOTS('',3,(#8015,#8016,#8017,#8018),
 .UNSPECIFIED.,.F.,.F.,(4,4),(0.,0.000876980038522527),.UNSPECIFIED.);
#672=B_SPLINE_CURVE_WITH_KNOTS('',3,(#8020,#8021,#8022,#8023),
 .UNSPECIFIED.,.F.,.F.,(4,4),(0.,0.000876980038522527),.UNSPECIFIED.);
#673=B_SPLINE_CURVE_WITH_KNOTS('',3,(#8104,#8105,#8106,#8107,#8108,#8109),
 .UNSPECIFIED.,.F.,.F.,(4,1,1,4),(-0.0376586249368312,-0.0177089806563706,
-0.00773415851614028,0.00224066362409002),.UNSPECIFIED.);
#674=B_SPLINE_CURVE_WITH_KNOTS('',3,(#8110,#8111,#8112,#8113,#8114,#8115),
 .UNSPECIFIED.,.F.,.F.,(4,1,1,4),(4.39785759961698E-16,0.0187757639234785,
0.0281636458852176,0.0375515278469566),.UNSPECIFIED.);
#675=B_SPLINE_CURVE_WITH_KNOTS('',3,(#8126,#8127,#8128,#8129,#8130,#8131,
#8132,#8133,#8134,#8135,#8136,#8137,#8138,#8139,#8140,#8141,#8142,#8143,
#8144,#8145,#8146,#8147),.UNSPECIFIED.,.F.,.F.,(4,1,1,1,1,1,1,1,1,1,1,1,
1,1,1,1,1,1,1,4),(0.,0.00451289465242826,0.00902578930485651,0.0135386839572848,
0.018051578609713,0.0203080259359271,0.0225644732621413,0.0270773679145695,
0.0293338152407837,0.0315902625669978,0.0338467098932119,0.036103157219426,
0.0406160518718543,0.0451289465242826,0.0496418411767108,0.0541547358291391,
0.0586676304815673,0.0631805251339956,0.0676934197864238,0.0722063144388521),
 .UNSPECIFIED.);
#676=B_SPLINE_CURVE_WITH_KNOTS('',3,(#8149,#8150,#8151,#8152,#8153,#8154),
 .UNSPECIFIED.,.F.,.F.,(4,1,1,4),(4.14598910758457E-16,0.00990633188871804,
0.0198126637774357,0.0396253275548709),.UNSPECIFIED.);
#677=B_SPLINE_CURVE_WITH_KNOTS('',3,(#8163,#8164,#8165,#8166,#8167),
 .UNSPECIFIED.,.F.,.F.,(4,1,4),(7.75791922889773E-18,0.0187679100601147,
0.0375358201202294),.UNSPECIFIED.);
#678=B_SPLINE_CURVE_WITH_KNOTS('',3,(#8171,#8172,#8173,#8174,#8175,#8176,
#8177,#8178,#8179),.UNSPECIFIED.,.F.,.F.,(4,1,1,1,1,1,4),(0.,0.00246792104240225,
0.00370188156360338,0.0049358420848045,0.00616980260600563,0.00740376312720676,
0.00987168416960901),.UNSPECIFIED.);
#679=B_SPLINE_CURVE_WITH_KNOTS('',3,(#8182,#8183,#8184,#8185,#8186,#8187,
#8188,#8189,#8190),.UNSPECIFIED.,.F.,.F.,(4,1,1,1,1,1,4),(4.03187682893047E-19,
0.00253597196642849,0.00380395794964274,0.00507194393285698,0.00633992991607123,
0.00760791589928547,0.010143887865714),.UNSPECIFIED.);
#680=B_SPLINE_CURVE_WITH_KNOTS('',3,(#8204,#8205,#8206,#8207),
 .UNSPECIFIED.,.F.,.F.,(4,4),(2.1900902092527E-7,0.0027185779941561),
 .UNSPECIFIED.);
#681=B_SPLINE_CURVE_WITH_KNOTS('',3,(#8211,#8212,#8213,#8214,#8215,#8216,
#8217,#8218,#8219,#8220,#8221,#8222,#8223,#8224,#8225,#8226,#8227,#8228,
#8229,#8230,#8231,#8232),.UNSPECIFIED.,.F.,.F.,(4,1,1,1,1,1,1,1,1,1,1,1,
1,1,1,1,1,1,1,4),(2.15427911492917E-7,0.00612092101240522,0.0122416265968989,
0.0183623321813927,0.0244830377658864,0.0306037433503801,0.0367244489348739,
0.0397848017271207,0.0428451545193676,0.0489658601038613,0.0520262128961082,
0.055086565688355,0.0612072712728488,0.0673279768573425,0.0703883296495894,
0.0734486824418362,0.0795693880263299,0.0856900936108237,0.0918107991953174,
0.0979315047798111),.UNSPECIFIED.);
#682=B_SPLINE_CURVE_WITH_KNOTS('',3,(#8234,#8235,#8236,#8237),
 .UNSPECIFIED.,.F.,.F.,(4,4),(2.15328326043877E-7,0.00271635611451793),
 .UNSPECIFIED.);
#683=B_SPLINE_CURVE_WITH_KNOTS('',3,(#8246,#8247,#8248,#8249,#8250,#8251,
#8252,#8253,#8254),.UNSPECIFIED.,.F.,.F.,(4,1,1,1,1,1,4),(0.,0.00248512918851248,
0.00372769378276871,0.00497025837702495,0.00621282297128119,0.00745538756553743,
0.0099405167540499),.UNSPECIFIED.);
#684=B_SPLINE_CURVE_WITH_KNOTS('',3,(#8259,#8260,#8261,#8262,#8263,#8264,
#8265,#8266,#8267),.UNSPECIFIED.,.F.,.F.,(4,1,1,1,1,1,4),(0.,0.00247246452692368,
0.00370869679038551,0.00494492905384735,0.00618116131730919,0.00741739358077102,
0.0098898581076947),.UNSPECIFIED.);
#685=B_SPLINE_CURVE_WITH_KNOTS('',3,(#8281,#8282,#8283,#8284,#8285,#8286,
#8287,#8288,#8289),.UNSPECIFIED.,.F.,.F.,(4,1,1,1,1,1,4),(4.33680868994202E-19,
0.00217116695540332,0.00325675043310498,0.00434233391080664,0.00542791738850829,
0.00651350086620995,0.00868466782161327),.UNSPECIFIED.);
#686=B_SPLINE_CURVE_WITH_KNOTS('',3,(#8293,#8294,#8295,#8296,#8297,#8298,
#8299,#8300,#8301),.UNSPECIFIED.,.F.,.F.,(4,1,1,1,1,1,4),(1.98874244301294E-16,
0.00217116695540802,0.00325675043311192,0.00434233391081583,0.00542791738851974,
0.00651350086622365,0.00868466782163146),.UNSPECIFIED.);
#687=B_SPLINE_CURVE_WITH_KNOTS('',3,(#8305,#8306,#8307,#8308,#8309,#8310,
#8311,#8312,#8313),.UNSPECIFIED.,.F.,.F.,(4,1,1,1,1,1,4),(2.94857387122129E-16,
0.00248512918850741,0.00372769378276096,0.00497025837701452,0.00621282297126808,
0.00745538756552163,0.00994051675402874),.UNSPECIFIED.);
#688=B_SPLINE_CURVE_WITH_KNOTS('',3,(#8323,#8324,#8325,#8326),
 .UNSPECIFIED.,.F.,.F.,(4,4),(0.,0.000678185781570246),.UNSPECIFIED.);
#689=B_SPLINE_CURVE_WITH_KNOTS('',3,(#8330,#8331,#8332,#8333,#8334,#8335,
#8336,#8337,#8338),.UNSPECIFIED.,.F.,.F.,(4,1,1,1,1,1,4),(7.152448122691E-18,
0.00214700943930209,0.00322051415895314,0.00429401887860418,0.00536752359825522,
0.00644102831790627,0.00858803775720835),.UNSPECIFIED.);
#690=B_SPLINE_CURVE_WITH_KNOTS('',3,(#8339,#8340,#8341,#8342,#8343,#8344,
#8345,#8346,#8347,#8348,#8349),.UNSPECIFIED.,.T.,.F.,(1,1,1,1,1,1,1,1,1,
1,1,1,1,1,1),(-0.00703767296465454,-0.00469178197643636,-0.00234589098821818,
0.,0.00234589098821818,0.00469178197643636,0.00703767296465454,0.00938356395287272,
0.0117294549410909,0.0140753459293091,0.0164212369175273,0.0187671279057454,
0.0211130188939636,0.0234589098821818,0.0258048008704),.UNSPECIFIED.);
#691=B_SPLINE_CURVE_WITH_KNOTS('',3,(#8381,#8382,#8383,#8384,#8385,#8386),
 .UNSPECIFIED.,.F.,.F.,(4,1,1,4),(4.30194153152991E-16,0.0195333936657401,
0.0293000904986099,0.0390667873314798),.UNSPECIFIED.);
#692=B_SPLINE_CURVE_WITH_KNOTS('',3,(#8390,#8391,#8392,#8393,#8394),
 .UNSPECIFIED.,.F.,.F.,(4,1,4),(1.16627099047498E-16,0.0187679100601151,
0.03753582012023),.UNSPECIFIED.);
#693=B_SPLINE_CURVE_WITH_KNOTS('',3,(#8401,#8402,#8403,#8404,#8405,#8406,
#8407,#8408,#8409,#8410,#8411,#8412,#8413,#8414,#8415,#8416,#8417,#8418,
#8419,#8420,#8421,#8422),.UNSPECIFIED.,.F.,.F.,(4,1,1,1,1,1,1,1,1,1,1,1,
1,1,1,1,1,1,1,4),(1.02803407384313E-16,0.00451289465242834,0.00902578930485658,
0.0135386839572848,0.0180515786097131,0.0203080259359272,0.0225644732621413,
0.0270773679145695,0.0293338152407837,0.0315902625669978,0.0338467098932119,
0.036103157219426,0.0406160518718543,0.0451289465242825,0.0496418411767107,
0.054154735829139,0.0586676304815672,0.0631805251339955,0.0676934197864237,
0.0722063144388519),.UNSPECIFIED.);
#694=B_SPLINE_CURVE_WITH_KNOTS('',3,(#8424,#8425,#8426,#8427,#8428,#8429),
 .UNSPECIFIED.,.F.,.F.,(4,1,1,4),(2.19892879980849E-16,0.018775763923479,
0.0281636458852184,0.0375515278469578),.UNSPECIFIED.);
#695=B_SPLINE_CURVE_WITH_KNOTS('',3,(#8433,#8434,#8435,#8436,#8437),
 .UNSPECIFIED.,.F.,.F.,(4,1,4),(0.,0.0195237738539724,0.0390475477079449),
 .UNSPECIFIED.);
#696=B_SPLINE_CURVE_WITH_KNOTS('',3,(#8462,#8463,#8464,#8465),
 .UNSPECIFIED.,.F.,.F.,(4,4),(4.39402408874622E-16,0.00271835452853781),
 .UNSPECIFIED.);
#697=B_SPLINE_CURVE_WITH_KNOTS('',3,(#8468,#8469,#8470,#8471,#8472,#8473,
#8474,#8475,#8476,#8477,#8478,#8479,#8480,#8481,#8482,#8483,#8484,#8485,
#8486,#8487,#8488,#8489),.UNSPECIFIED.,.F.,.F.,(4,1,1,1,1,1,1,1,1,1,1,1,
1,1,1,1,1,1,1,4),(2.52579550652517E-17,0.00612070517530055,0.0122414103506011,
0.0183621155259016,0.0244828207012021,0.0306035258765026,0.0367242310518032,
0.0397845836394534,0.0428449362271037,0.0489656414024042,0.0520259939900545,
0.0550863465777047,0.0612070517530053,0.0673277569283058,0.070388109515956,
0.0734484621036063,0.0795691672789068,0.0856898724542074,0.0918105776295079,
0.0979312828048084),.UNSPECIFIED.);
#698=B_SPLINE_CURVE_WITH_KNOTS('',3,(#8491,#8492,#8493,#8494),
 .UNSPECIFIED.,.F.,.F.,(4,4),(0.,0.00271613773257923),.UNSPECIFIED.);
#699=ORIENTED_EDGE('',*,*,#1869,.F.);
#700=ORIENTED_EDGE('',*,*,#1870,.T.);
#701=ORIENTED_EDGE('',*,*,#1871,.T.);
#702=ORIENTED_EDGE('',*,*,#1872,.T.);
#703=ORIENTED_EDGE('',*,*,#1873,.F.);
#704=ORIENTED_EDGE('',*,*,#1874,.F.);
#705=ORIENTED_EDGE('',*,*,#1875,.T.);
#706=ORIENTED_EDGE('',*,*,#1876,.T.);
#707=ORIENTED_EDGE('',*,*,#1869,.T.);
#708=ORIENTED_EDGE('',*,*,#1877,.F.);
#709=ORIENTED_EDGE('',*,*,#1878,.F.);
#710=ORIENTED_EDGE('',*,*,#1879,.T.);
#711=ORIENTED_EDGE('',*,*,#1880,.T.);
#712=ORIENTED_EDGE('',*,*,#1874,.T.);
#713=ORIENTED_EDGE('',*,*,#1881,.F.);
#714=ORIENTED_EDGE('',*,*,#1882,.F.);
#715=ORIENTED_EDGE('',*,*,#1883,.T.);
#716=ORIENTED_EDGE('',*,*,#1884,.T.);
#717=ORIENTED_EDGE('',*,*,#1878,.T.);
#718=ORIENTED_EDGE('',*,*,#1885,.F.);
#719=ORIENTED_EDGE('',*,*,#1886,.F.);
#720=ORIENTED_EDGE('',*,*,#1887,.T.);
#721=ORIENTED_EDGE('',*,*,#1888,.T.);
#722=ORIENTED_EDGE('',*,*,#1882,.T.);
#723=ORIENTED_EDGE('',*,*,#1889,.F.);
#724=ORIENTED_EDGE('',*,*,#1872,.F.);
#725=ORIENTED_EDGE('',*,*,#1890,.T.);
#726=ORIENTED_EDGE('',*,*,#1891,.T.);
#727=ORIENTED_EDGE('',*,*,#1886,.T.);
#728=ORIENTED_EDGE('',*,*,#1892,.F.);
#729=ORIENTED_EDGE('',*,*,#1893,.T.);
#730=ORIENTED_EDGE('',*,*,#1873,.T.);
#731=ORIENTED_EDGE('',*,*,#1892,.T.);
#732=ORIENTED_EDGE('',*,*,#1889,.T.);
#733=ORIENTED_EDGE('',*,*,#1885,.T.);
#734=ORIENTED_EDGE('',*,*,#1881,.T.);
#735=ORIENTED_EDGE('',*,*,#1877,.T.);
#736=ORIENTED_EDGE('',*,*,#1894,.T.);
#737=ORIENTED_EDGE('',*,*,#1895,.T.);
#738=ORIENTED_EDGE('',*,*,#1896,.T.);
#739=ORIENTED_EDGE('',*,*,#1891,.F.);
#740=ORIENTED_EDGE('',*,*,#1897,.F.);
#741=ORIENTED_EDGE('',*,*,#1887,.F.);
#742=ORIENTED_EDGE('',*,*,#1898,.F.);
#743=ORIENTED_EDGE('',*,*,#1890,.F.);
#744=ORIENTED_EDGE('',*,*,#1871,.F.);
#745=ORIENTED_EDGE('',*,*,#1888,.F.);
#746=ORIENTED_EDGE('',*,*,#1899,.F.);
#747=ORIENTED_EDGE('',*,*,#1883,.F.);
#748=ORIENTED_EDGE('',*,*,#1884,.F.);
#749=ORIENTED_EDGE('',*,*,#1900,.F.);
#750=ORIENTED_EDGE('',*,*,#1879,.F.);
#751=ORIENTED_EDGE('',*,*,#1901,.F.);
#752=ORIENTED_EDGE('',*,*,#1875,.F.);
#753=ORIENTED_EDGE('',*,*,#1880,.F.);
#754=ORIENTED_EDGE('',*,*,#1902,.F.);
#755=ORIENTED_EDGE('',*,*,#1870,.F.);
#756=ORIENTED_EDGE('',*,*,#1876,.F.);
#757=ORIENTED_EDGE('',*,*,#1899,.T.);
#758=ORIENTED_EDGE('',*,*,#1897,.T.);
#759=ORIENTED_EDGE('',*,*,#1898,.T.);
#760=ORIENTED_EDGE('',*,*,#1902,.T.);
#761=ORIENTED_EDGE('',*,*,#1901,.T.);
#762=ORIENTED_EDGE('',*,*,#1900,.T.);
#763=ORIENTED_EDGE('',*,*,#1893,.F.);
#764=ORIENTED_EDGE('',*,*,#1895,.F.);
#765=ORIENTED_EDGE('',*,*,#1894,.F.);
#766=ORIENTED_EDGE('',*,*,#1896,.F.);
#767=ORIENTED_EDGE('',*,*,#1903,.T.);
#768=ORIENTED_EDGE('',*,*,#1904,.F.);
#769=ORIENTED_EDGE('',*,*,#1905,.F.);
#770=ORIENTED_EDGE('',*,*,#1906,.T.);
#771=ORIENTED_EDGE('',*,*,#1903,.F.);
#772=ORIENTED_EDGE('',*,*,#1905,.T.);
#773=ORIENTED_EDGE('',*,*,#1904,.T.);
#774=ORIENTED_EDGE('',*,*,#1906,.F.);
#775=ORIENTED_EDGE('',*,*,#1907,.T.);
#776=ORIENTED_EDGE('',*,*,#1908,.F.);
#777=ORIENTED_EDGE('',*,*,#1909,.F.);
#778=ORIENTED_EDGE('',*,*,#1910,.T.);
#779=ORIENTED_EDGE('',*,*,#1911,.T.);
#780=ORIENTED_EDGE('',*,*,#1912,.F.);
#781=ORIENTED_EDGE('',*,*,#1913,.F.);
#782=ORIENTED_EDGE('',*,*,#1908,.T.);
#783=ORIENTED_EDGE('',*,*,#1914,.T.);
#784=ORIENTED_EDGE('',*,*,#1915,.F.);
#785=ORIENTED_EDGE('',*,*,#1916,.F.);
#786=ORIENTED_EDGE('',*,*,#1912,.T.);
#787=ORIENTED_EDGE('',*,*,#1917,.T.);
#788=ORIENTED_EDGE('',*,*,#1910,.F.);
#789=ORIENTED_EDGE('',*,*,#1918,.F.);
#790=ORIENTED_EDGE('',*,*,#1915,.T.);
#791=ORIENTED_EDGE('',*,*,#1909,.T.);
#792=ORIENTED_EDGE('',*,*,#1913,.T.);
#793=ORIENTED_EDGE('',*,*,#1916,.T.);
#794=ORIENTED_EDGE('',*,*,#1918,.T.);
#795=ORIENTED_EDGE('',*,*,#1907,.F.);
#796=ORIENTED_EDGE('',*,*,#1917,.F.);
#797=ORIENTED_EDGE('',*,*,#1914,.F.);
#798=ORIENTED_EDGE('',*,*,#1911,.F.);
#799=ORIENTED_EDGE('',*,*,#1919,.T.);
#800=ORIENTED_EDGE('',*,*,#1920,.T.);
#801=ORIENTED_EDGE('',*,*,#1921,.T.);
#802=ORIENTED_EDGE('',*,*,#1922,.T.);
#803=ORIENTED_EDGE('',*,*,#1923,.F.);
#804=ORIENTED_EDGE('',*,*,#1924,.F.);
#805=ORIENTED_EDGE('',*,*,#1925,.T.);
#806=ORIENTED_EDGE('',*,*,#1926,.F.);
#807=ORIENTED_EDGE('',*,*,#1919,.F.);
#808=ORIENTED_EDGE('',*,*,#1927,.F.);
#809=ORIENTED_EDGE('',*,*,#1928,.F.);
#810=ORIENTED_EDGE('',*,*,#1928,.T.);
#811=ORIENTED_EDGE('',*,*,#1929,.F.);
#812=ORIENTED_EDGE('',*,*,#1929,.T.);
#813=ORIENTED_EDGE('',*,*,#1930,.F.);
#814=ORIENTED_EDGE('',*,*,#1930,.T.);
#815=ORIENTED_EDGE('',*,*,#1931,.F.);
#816=ORIENTED_EDGE('',*,*,#1931,.T.);
#817=ORIENTED_EDGE('',*,*,#1932,.F.);
#818=ORIENTED_EDGE('',*,*,#1932,.T.);
#819=ORIENTED_EDGE('',*,*,#1933,.F.);
#820=ORIENTED_EDGE('',*,*,#1933,.T.);
#821=ORIENTED_EDGE('',*,*,#1934,.F.);
#822=ORIENTED_EDGE('',*,*,#1934,.T.);
#823=ORIENTED_EDGE('',*,*,#1935,.F.);
#824=ORIENTED_EDGE('',*,*,#1935,.T.);
#825=ORIENTED_EDGE('',*,*,#1936,.F.);
#826=ORIENTED_EDGE('',*,*,#1936,.T.);
#827=ORIENTED_EDGE('',*,*,#1937,.F.);
#828=ORIENTED_EDGE('',*,*,#1937,.T.);
#829=ORIENTED_EDGE('',*,*,#1938,.F.);
#830=ORIENTED_EDGE('',*,*,#1938,.T.);
#831=ORIENTED_EDGE('',*,*,#1939,.F.);
#832=ORIENTED_EDGE('',*,*,#1939,.T.);
#833=ORIENTED_EDGE('',*,*,#1940,.F.);
#834=ORIENTED_EDGE('',*,*,#1940,.T.);
#835=ORIENTED_EDGE('',*,*,#1941,.F.);
#836=ORIENTED_EDGE('',*,*,#1941,.T.);
#837=ORIENTED_EDGE('',*,*,#1942,.F.);
#838=ORIENTED_EDGE('',*,*,#1942,.T.);
#839=ORIENTED_EDGE('',*,*,#1943,.F.);
#840=ORIENTED_EDGE('',*,*,#1943,.T.);
#841=ORIENTED_EDGE('',*,*,#1922,.F.);
#842=ORIENTED_EDGE('',*,*,#1923,.T.);
#843=ORIENTED_EDGE('',*,*,#1925,.F.);
#844=ORIENTED_EDGE('',*,*,#1927,.T.);
#845=ORIENTED_EDGE('',*,*,#1921,.F.);
#846=ORIENTED_EDGE('',*,*,#1944,.T.);
#847=ORIENTED_EDGE('',*,*,#1944,.F.);
#848=ORIENTED_EDGE('',*,*,#1920,.F.);
#849=ORIENTED_EDGE('',*,*,#1924,.T.);
#850=ORIENTED_EDGE('',*,*,#1945,.F.);
#851=ORIENTED_EDGE('',*,*,#1945,.T.);
#852=ORIENTED_EDGE('',*,*,#1946,.F.);
#853=ORIENTED_EDGE('',*,*,#1926,.T.);
#854=ORIENTED_EDGE('',*,*,#1946,.T.);
#855=ORIENTED_EDGE('',*,*,#1947,.F.);
#856=ORIENTED_EDGE('',*,*,#1948,.T.);
#857=ORIENTED_EDGE('',*,*,#1949,.T.);
#858=ORIENTED_EDGE('',*,*,#1950,.F.);
#859=ORIENTED_EDGE('',*,*,#1947,.T.);
#860=ORIENTED_EDGE('',*,*,#1949,.F.);
#861=ORIENTED_EDGE('',*,*,#1948,.F.);
#862=ORIENTED_EDGE('',*,*,#1950,.T.);
#863=ORIENTED_EDGE('',*,*,#1951,.T.);
#864=ORIENTED_EDGE('',*,*,#1952,.T.);
#865=ORIENTED_EDGE('',*,*,#1953,.F.);
#866=ORIENTED_EDGE('',*,*,#1954,.T.);
#867=ORIENTED_EDGE('',*,*,#1955,.T.);
#868=ORIENTED_EDGE('',*,*,#1956,.F.);
#869=ORIENTED_EDGE('',*,*,#1957,.F.);
#870=ORIENTED_EDGE('',*,*,#1954,.F.);
#871=ORIENTED_EDGE('',*,*,#1958,.T.);
#872=ORIENTED_EDGE('',*,*,#1952,.F.);
#873=ORIENTED_EDGE('',*,*,#1959,.F.);
#874=ORIENTED_EDGE('',*,*,#1960,.F.);
#875=ORIENTED_EDGE('',*,*,#1961,.T.);
#876=ORIENTED_EDGE('',*,*,#1962,.F.);
#877=ORIENTED_EDGE('',*,*,#1955,.F.);
#878=ORIENTED_EDGE('',*,*,#1963,.F.);
#879=ORIENTED_EDGE('',*,*,#1964,.T.);
#880=ORIENTED_EDGE('',*,*,#1965,.F.);
#881=ORIENTED_EDGE('',*,*,#1958,.F.);
#882=ORIENTED_EDGE('',*,*,#1966,.F.);
#883=ORIENTED_EDGE('',*,*,#1957,.T.);
#884=ORIENTED_EDGE('',*,*,#1967,.F.);
#885=ORIENTED_EDGE('',*,*,#1968,.F.);
#886=ORIENTED_EDGE('',*,*,#1969,.F.);
#887=ORIENTED_EDGE('',*,*,#1959,.T.);
#888=ORIENTED_EDGE('',*,*,#1970,.F.);
#889=ORIENTED_EDGE('',*,*,#1971,.F.);
#890=ORIENTED_EDGE('',*,*,#1972,.F.);
#891=ORIENTED_EDGE('',*,*,#1973,.F.);
#892=ORIENTED_EDGE('',*,*,#1974,.F.);
#893=ORIENTED_EDGE('',*,*,#1964,.F.);
#894=ORIENTED_EDGE('',*,*,#1975,.F.);
#895=ORIENTED_EDGE('',*,*,#1976,.F.);
#896=ORIENTED_EDGE('',*,*,#1977,.F.);
#897=ORIENTED_EDGE('',*,*,#1961,.F.);
#898=ORIENTED_EDGE('',*,*,#1978,.F.);
#899=ORIENTED_EDGE('',*,*,#1979,.F.);
#900=ORIENTED_EDGE('',*,*,#1978,.T.);
#901=ORIENTED_EDGE('',*,*,#1980,.F.);
#902=ORIENTED_EDGE('',*,*,#1974,.T.);
#903=ORIENTED_EDGE('',*,*,#1981,.F.);
#904=ORIENTED_EDGE('',*,*,#1982,.F.);
#905=ORIENTED_EDGE('',*,*,#1983,.F.);
#906=ORIENTED_EDGE('',*,*,#1984,.T.);
#907=ORIENTED_EDGE('',*,*,#1985,.F.);
#908=ORIENTED_EDGE('',*,*,#1986,.T.);
#909=ORIENTED_EDGE('',*,*,#1987,.F.);
#910=ORIENTED_EDGE('',*,*,#1988,.T.);
#911=ORIENTED_EDGE('',*,*,#1989,.F.);
#912=ORIENTED_EDGE('',*,*,#1987,.T.);
#913=ORIENTED_EDGE('',*,*,#1990,.F.);
#914=ORIENTED_EDGE('',*,*,#1982,.T.);
#915=ORIENTED_EDGE('',*,*,#1991,.F.);
#916=ORIENTED_EDGE('',*,*,#1992,.T.);
#917=ORIENTED_EDGE('',*,*,#1993,.F.);
#918=ORIENTED_EDGE('',*,*,#1994,.T.);
#919=ORIENTED_EDGE('',*,*,#1995,.F.);
#920=ORIENTED_EDGE('',*,*,#1996,.T.);
#921=ORIENTED_EDGE('',*,*,#1997,.F.);
#922=ORIENTED_EDGE('',*,*,#1998,.F.);
#923=ORIENTED_EDGE('',*,*,#1996,.F.);
#924=ORIENTED_EDGE('',*,*,#1999,.T.);
#925=ORIENTED_EDGE('',*,*,#1991,.T.);
#926=ORIENTED_EDGE('',*,*,#2000,.T.);
#927=ORIENTED_EDGE('',*,*,#1998,.T.);
#928=ORIENTED_EDGE('',*,*,#2001,.T.);
#929=ORIENTED_EDGE('',*,*,#1984,.F.);
#930=ORIENTED_EDGE('',*,*,#2002,.T.);
#931=ORIENTED_EDGE('',*,*,#2003,.F.);
#932=ORIENTED_EDGE('',*,*,#2004,.F.);
#933=ORIENTED_EDGE('',*,*,#1971,.T.);
#934=ORIENTED_EDGE('',*,*,#2005,.F.);
#935=ORIENTED_EDGE('',*,*,#2006,.F.);
#936=ORIENTED_EDGE('',*,*,#2007,.F.);
#937=ORIENTED_EDGE('',*,*,#1968,.T.);
#938=ORIENTED_EDGE('',*,*,#2008,.F.);
#939=ORIENTED_EDGE('',*,*,#2007,.T.);
#940=ORIENTED_EDGE('',*,*,#2009,.T.);
#941=ORIENTED_EDGE('',*,*,#2005,.T.);
#942=ORIENTED_EDGE('',*,*,#2010,.T.);
#943=ORIENTED_EDGE('',*,*,#2004,.T.);
#944=ORIENTED_EDGE('',*,*,#2011,.T.);
#945=ORIENTED_EDGE('',*,*,#1993,.T.);
#946=ORIENTED_EDGE('',*,*,#2012,.T.);
#947=ORIENTED_EDGE('',*,*,#1975,.T.);
#948=ORIENTED_EDGE('',*,*,#1966,.T.);
#949=ORIENTED_EDGE('',*,*,#1960,.T.);
#950=ORIENTED_EDGE('',*,*,#1972,.T.);
#951=ORIENTED_EDGE('',*,*,#2013,.F.);
#952=ORIENTED_EDGE('',*,*,#2008,.T.);
#953=ORIENTED_EDGE('',*,*,#1967,.T.);
#954=ORIENTED_EDGE('',*,*,#1956,.T.);
#955=ORIENTED_EDGE('',*,*,#1962,.T.);
#956=ORIENTED_EDGE('',*,*,#1977,.T.);
#957=ORIENTED_EDGE('',*,*,#2014,.F.);
#958=ORIENTED_EDGE('',*,*,#1985,.T.);
#959=ORIENTED_EDGE('',*,*,#2015,.T.);
#960=ORIENTED_EDGE('',*,*,#1953,.T.);
#961=ORIENTED_EDGE('',*,*,#1965,.T.);
#962=ORIENTED_EDGE('',*,*,#1980,.T.);
#963=ORIENTED_EDGE('',*,*,#1963,.T.);
#964=ORIENTED_EDGE('',*,*,#2016,.T.);
#965=ORIENTED_EDGE('',*,*,#2015,.F.);
#966=ORIENTED_EDGE('',*,*,#2017,.T.);
#967=ORIENTED_EDGE('',*,*,#2010,.F.);
#968=ORIENTED_EDGE('',*,*,#1970,.T.);
#969=ORIENTED_EDGE('',*,*,#1951,.F.);
#970=ORIENTED_EDGE('',*,*,#1969,.T.);
#971=ORIENTED_EDGE('',*,*,#2018,.T.);
#972=ORIENTED_EDGE('',*,*,#2017,.F.);
#973=ORIENTED_EDGE('',*,*,#2011,.F.);
#974=ORIENTED_EDGE('',*,*,#2003,.T.);
#975=ORIENTED_EDGE('',*,*,#2009,.F.);
#976=ORIENTED_EDGE('',*,*,#2006,.T.);
#977=ORIENTED_EDGE('',*,*,#2013,.T.);
#978=ORIENTED_EDGE('',*,*,#1988,.F.);
#979=ORIENTED_EDGE('',*,*,#1989,.T.);
#980=ORIENTED_EDGE('',*,*,#1981,.T.);
#981=ORIENTED_EDGE('',*,*,#2001,.F.);
#982=ORIENTED_EDGE('',*,*,#1997,.T.);
#983=ORIENTED_EDGE('',*,*,#2000,.F.);
#984=ORIENTED_EDGE('',*,*,#1994,.F.);
#985=ORIENTED_EDGE('',*,*,#2018,.F.);
#986=ORIENTED_EDGE('',*,*,#1999,.F.);
#987=ORIENTED_EDGE('',*,*,#1995,.T.);
#988=ORIENTED_EDGE('',*,*,#2002,.F.);
#989=ORIENTED_EDGE('',*,*,#1983,.T.);
#990=ORIENTED_EDGE('',*,*,#1990,.T.);
#991=ORIENTED_EDGE('',*,*,#1986,.F.);
#992=ORIENTED_EDGE('',*,*,#2014,.T.);
#993=ORIENTED_EDGE('',*,*,#1976,.T.);
#994=ORIENTED_EDGE('',*,*,#1979,.T.);
#995=ORIENTED_EDGE('',*,*,#1973,.T.);
#996=ORIENTED_EDGE('',*,*,#2012,.F.);
#997=ORIENTED_EDGE('',*,*,#1992,.F.);
#998=ORIENTED_EDGE('',*,*,#2016,.F.);
#999=ORIENTED_EDGE('',*,*,#2019,.T.);
#1000=ORIENTED_EDGE('',*,*,#2020,.T.);
#1001=ORIENTED_EDGE('',*,*,#2021,.T.);
#1002=ORIENTED_EDGE('',*,*,#2022,.T.);
#1003=ORIENTED_EDGE('',*,*,#2023,.T.);
#1004=ORIENTED_EDGE('',*,*,#2024,.T.);
#1005=ORIENTED_EDGE('',*,*,#2025,.T.);
#1006=ORIENTED_EDGE('',*,*,#2026,.T.);
#1007=ORIENTED_EDGE('',*,*,#2027,.F.);
#1008=ORIENTED_EDGE('',*,*,#2028,.T.);
#1009=ORIENTED_EDGE('',*,*,#2029,.T.);
#1010=ORIENTED_EDGE('',*,*,#2030,.T.);
#1011=ORIENTED_EDGE('',*,*,#2031,.T.);
#1012=ORIENTED_EDGE('',*,*,#2032,.T.);
#1013=ORIENTED_EDGE('',*,*,#2033,.F.);
#1014=ORIENTED_EDGE('',*,*,#2034,.T.);
#1015=ORIENTED_EDGE('',*,*,#2035,.F.);
#1016=ORIENTED_EDGE('',*,*,#2036,.T.);
#1017=ORIENTED_EDGE('',*,*,#2037,.T.);
#1018=ORIENTED_EDGE('',*,*,#2038,.T.);
#1019=ORIENTED_EDGE('',*,*,#2039,.T.);
#1020=ORIENTED_EDGE('',*,*,#2040,.T.);
#1021=ORIENTED_EDGE('',*,*,#2041,.T.);
#1022=ORIENTED_EDGE('',*,*,#2042,.T.);
#1023=ORIENTED_EDGE('',*,*,#2043,.F.);
#1024=ORIENTED_EDGE('',*,*,#2044,.T.);
#1025=ORIENTED_EDGE('',*,*,#2045,.F.);
#1026=ORIENTED_EDGE('',*,*,#2046,.F.);
#1027=ORIENTED_EDGE('',*,*,#2047,.T.);
#1028=ORIENTED_EDGE('',*,*,#2048,.F.);
#1029=ORIENTED_EDGE('',*,*,#2049,.F.);
#1030=ORIENTED_EDGE('',*,*,#2050,.F.);
#1031=ORIENTED_EDGE('',*,*,#2051,.F.);
#1032=ORIENTED_EDGE('',*,*,#2052,.F.);
#1033=ORIENTED_EDGE('',*,*,#2053,.F.);
#1034=ORIENTED_EDGE('',*,*,#2054,.T.);
#1035=ORIENTED_EDGE('',*,*,#2052,.T.);
#1036=ORIENTED_EDGE('',*,*,#2055,.T.);
#1037=ORIENTED_EDGE('',*,*,#2044,.F.);
#1038=ORIENTED_EDGE('',*,*,#2056,.T.);
#1039=ORIENTED_EDGE('',*,*,#2057,.T.);
#1040=ORIENTED_EDGE('',*,*,#2058,.T.);
#1041=ORIENTED_EDGE('',*,*,#2059,.T.);
#1042=ORIENTED_EDGE('',*,*,#2060,.T.);
#1043=ORIENTED_EDGE('',*,*,#2059,.F.);
#1044=ORIENTED_EDGE('',*,*,#2061,.T.);
#1045=ORIENTED_EDGE('',*,*,#2046,.T.);
#1046=ORIENTED_EDGE('',*,*,#2062,.T.);
#1047=ORIENTED_EDGE('',*,*,#2023,.F.);
#1048=ORIENTED_EDGE('',*,*,#2063,.T.);
#1049=ORIENTED_EDGE('',*,*,#2039,.F.);
#1050=ORIENTED_EDGE('',*,*,#2064,.T.);
#1051=ORIENTED_EDGE('',*,*,#2041,.F.);
#1052=ORIENTED_EDGE('',*,*,#2065,.T.);
#1053=ORIENTED_EDGE('',*,*,#2032,.F.);
#1054=ORIENTED_EDGE('',*,*,#2066,.T.);
#1055=ORIENTED_EDGE('',*,*,#2036,.F.);
#1056=ORIENTED_EDGE('',*,*,#2067,.T.);
#1057=ORIENTED_EDGE('',*,*,#2019,.F.);
#1058=ORIENTED_EDGE('',*,*,#2068,.F.);
#1059=ORIENTED_EDGE('',*,*,#2028,.F.);
#1060=ORIENTED_EDGE('',*,*,#2069,.T.);
#1061=ORIENTED_EDGE('',*,*,#2038,.F.);
#1062=ORIENTED_EDGE('',*,*,#2070,.F.);
#1063=ORIENTED_EDGE('',*,*,#2071,.F.);
#1064=ORIENTED_EDGE('',*,*,#2054,.F.);
#1065=ORIENTED_EDGE('',*,*,#2072,.F.);
#1066=ORIENTED_EDGE('',*,*,#2034,.F.);
#1067=ORIENTED_EDGE('',*,*,#2073,.F.);
#1068=ORIENTED_EDGE('',*,*,#2021,.F.);
#1069=ORIENTED_EDGE('',*,*,#2074,.F.);
#1070=ORIENTED_EDGE('',*,*,#2057,.F.);
#1071=ORIENTED_EDGE('',*,*,#2075,.T.);
#1072=ORIENTED_EDGE('',*,*,#2076,.T.);
#1073=ORIENTED_EDGE('',*,*,#2077,.T.);
#1074=ORIENTED_EDGE('',*,*,#2078,.T.);
#1075=ORIENTED_EDGE('',*,*,#2079,.T.);
#1076=ORIENTED_EDGE('',*,*,#2080,.T.);
#1077=ORIENTED_EDGE('',*,*,#2081,.T.);
#1078=ORIENTED_EDGE('',*,*,#2082,.T.);
#1079=ORIENTED_EDGE('',*,*,#2083,.T.);
#1080=ORIENTED_EDGE('',*,*,#2084,.T.);
#1081=ORIENTED_EDGE('',*,*,#2085,.T.);
#1082=ORIENTED_EDGE('',*,*,#2086,.T.);
#1083=ORIENTED_EDGE('',*,*,#2087,.T.);
#1084=ORIENTED_EDGE('',*,*,#2088,.T.);
#1085=ORIENTED_EDGE('',*,*,#2089,.T.);
#1086=ORIENTED_EDGE('',*,*,#2090,.T.);
#1087=ORIENTED_EDGE('',*,*,#2091,.T.);
#1088=ORIENTED_EDGE('',*,*,#2092,.T.);
#1089=ORIENTED_EDGE('',*,*,#2093,.T.);
#1090=ORIENTED_EDGE('',*,*,#2094,.T.);
#1091=ORIENTED_EDGE('',*,*,#2095,.T.);
#1092=ORIENTED_EDGE('',*,*,#2096,.T.);
#1093=ORIENTED_EDGE('',*,*,#2097,.T.);
#1094=ORIENTED_EDGE('',*,*,#2098,.F.);
#1095=ORIENTED_EDGE('',*,*,#2099,.T.);
#1096=ORIENTED_EDGE('',*,*,#2100,.T.);
#1097=ORIENTED_EDGE('',*,*,#2101,.T.);
#1098=ORIENTED_EDGE('',*,*,#2102,.T.);
#1099=ORIENTED_EDGE('',*,*,#2103,.T.);
#1100=ORIENTED_EDGE('',*,*,#2104,.T.);
#1101=ORIENTED_EDGE('',*,*,#2105,.T.);
#1102=ORIENTED_EDGE('',*,*,#2106,.T.);
#1103=ORIENTED_EDGE('',*,*,#2107,.T.);
#1104=ORIENTED_EDGE('',*,*,#2108,.T.);
#1105=ORIENTED_EDGE('',*,*,#2109,.T.);
#1106=ORIENTED_EDGE('',*,*,#2110,.T.);
#1107=ORIENTED_EDGE('',*,*,#2111,.T.);
#1108=ORIENTED_EDGE('',*,*,#2112,.F.);
#1109=ORIENTED_EDGE('',*,*,#2113,.T.);
#1110=ORIENTED_EDGE('',*,*,#2114,.T.);
#1111=ORIENTED_EDGE('',*,*,#2115,.T.);
#1112=ORIENTED_EDGE('',*,*,#2116,.T.);
#1113=ORIENTED_EDGE('',*,*,#2117,.T.);
#1114=ORIENTED_EDGE('',*,*,#2118,.T.);
#1115=ORIENTED_EDGE('',*,*,#2119,.T.);
#1116=ORIENTED_EDGE('',*,*,#2120,.T.);
#1117=ORIENTED_EDGE('',*,*,#2121,.T.);
#1118=ORIENTED_EDGE('',*,*,#2122,.T.);
#1119=ORIENTED_EDGE('',*,*,#2123,.T.);
#1120=ORIENTED_EDGE('',*,*,#2124,.T.);
#1121=ORIENTED_EDGE('',*,*,#2125,.T.);
#1122=ORIENTED_EDGE('',*,*,#2126,.T.);
#1123=ORIENTED_EDGE('',*,*,#2127,.T.);
#1124=ORIENTED_EDGE('',*,*,#2128,.T.);
#1125=ORIENTED_EDGE('',*,*,#2129,.T.);
#1126=ORIENTED_EDGE('',*,*,#2130,.T.);
#1127=ORIENTED_EDGE('',*,*,#2131,.T.);
#1128=ORIENTED_EDGE('',*,*,#2132,.T.);
#1129=ORIENTED_EDGE('',*,*,#2133,.T.);
#1130=ORIENTED_EDGE('',*,*,#2134,.T.);
#1131=ORIENTED_EDGE('',*,*,#2135,.T.);
#1132=ORIENTED_EDGE('',*,*,#2136,.T.);
#1133=ORIENTED_EDGE('',*,*,#2049,.T.);
#1134=ORIENTED_EDGE('',*,*,#2137,.T.);
#1135=ORIENTED_EDGE('',*,*,#2138,.T.);
#1136=ORIENTED_EDGE('',*,*,#2139,.T.);
#1137=ORIENTED_EDGE('',*,*,#2140,.T.);
#1138=ORIENTED_EDGE('',*,*,#2141,.T.);
#1139=ORIENTED_EDGE('',*,*,#2142,.F.);
#1140=ORIENTED_EDGE('',*,*,#2143,.T.);
#1141=ORIENTED_EDGE('',*,*,#2144,.T.);
#1142=ORIENTED_EDGE('',*,*,#2108,.F.);
#1143=ORIENTED_EDGE('',*,*,#2145,.T.);
#1144=ORIENTED_EDGE('',*,*,#2098,.T.);
#1145=ORIENTED_EDGE('',*,*,#2146,.T.);
#1146=ORIENTED_EDGE('',*,*,#2047,.F.);
#1147=ORIENTED_EDGE('',*,*,#2147,.T.);
#1148=ORIENTED_EDGE('',*,*,#2148,.T.);
#1149=ORIENTED_EDGE('',*,*,#2149,.T.);
#1150=ORIENTED_EDGE('',*,*,#2150,.T.);
#1151=ORIENTED_EDGE('',*,*,#2151,.T.);
#1152=ORIENTED_EDGE('',*,*,#2152,.T.);
#1153=ORIENTED_EDGE('',*,*,#2153,.T.);
#1154=ORIENTED_EDGE('',*,*,#2154,.T.);
#1155=ORIENTED_EDGE('',*,*,#2152,.F.);
#1156=ORIENTED_EDGE('',*,*,#2155,.T.);
#1157=ORIENTED_EDGE('',*,*,#2112,.T.);
#1158=ORIENTED_EDGE('',*,*,#2156,.T.);
#1159=ORIENTED_EDGE('',*,*,#2102,.F.);
#1160=ORIENTED_EDGE('',*,*,#2157,.T.);
#1161=ORIENTED_EDGE('',*,*,#2142,.T.);
#1162=ORIENTED_EDGE('',*,*,#2158,.T.);
#1163=ORIENTED_EDGE('',*,*,#2159,.T.);
#1164=ORIENTED_EDGE('',*,*,#2160,.T.);
#1165=ORIENTED_EDGE('',*,*,#2161,.T.);
#1166=ORIENTED_EDGE('',*,*,#2162,.T.);
#1167=ORIENTED_EDGE('',*,*,#2163,.F.);
#1168=ORIENTED_EDGE('',*,*,#2164,.T.);
#1169=ORIENTED_EDGE('',*,*,#2165,.T.);
#1170=ORIENTED_EDGE('',*,*,#2166,.T.);
#1171=ORIENTED_EDGE('',*,*,#2161,.F.);
#1172=ORIENTED_EDGE('',*,*,#2167,.T.);
#1173=ORIENTED_EDGE('',*,*,#2168,.T.);
#1174=ORIENTED_EDGE('',*,*,#2169,.T.);
#1175=ORIENTED_EDGE('',*,*,#2170,.T.);
#1176=ORIENTED_EDGE('',*,*,#2171,.T.);
#1177=ORIENTED_EDGE('',*,*,#2172,.T.);
#1178=ORIENTED_EDGE('',*,*,#2173,.T.);
#1179=ORIENTED_EDGE('',*,*,#2168,.F.);
#1180=ORIENTED_EDGE('',*,*,#2174,.T.);
#1181=ORIENTED_EDGE('',*,*,#2163,.T.);
#1182=ORIENTED_EDGE('',*,*,#2175,.T.);
#1183=ORIENTED_EDGE('',*,*,#2176,.T.);
#1184=ORIENTED_EDGE('',*,*,#2177,.T.);
#1185=ORIENTED_EDGE('',*,*,#2172,.F.);
#1186=ORIENTED_EDGE('',*,*,#2178,.T.);
#1187=ORIENTED_EDGE('',*,*,#2179,.T.);
#1188=ORIENTED_EDGE('',*,*,#2180,.T.);
#1189=ORIENTED_EDGE('',*,*,#2181,.T.);
#1190=ORIENTED_EDGE('',*,*,#2182,.T.);
#1191=ORIENTED_EDGE('',*,*,#2183,.T.);
#1192=ORIENTED_EDGE('',*,*,#2184,.T.);
#1193=ORIENTED_EDGE('',*,*,#2185,.F.);
#1194=ORIENTED_EDGE('',*,*,#2186,.T.);
#1195=ORIENTED_EDGE('',*,*,#2187,.T.);
#1196=ORIENTED_EDGE('',*,*,#2188,.T.);
#1197=ORIENTED_EDGE('',*,*,#2189,.T.);
#1198=ORIENTED_EDGE('',*,*,#2190,.T.);
#1199=ORIENTED_EDGE('',*,*,#2183,.F.);
#1200=ORIENTED_EDGE('',*,*,#2191,.T.);
#1201=ORIENTED_EDGE('',*,*,#2192,.T.);
#1202=ORIENTED_EDGE('',*,*,#2193,.T.);
#1203=ORIENTED_EDGE('',*,*,#2187,.F.);
#1204=ORIENTED_EDGE('',*,*,#2194,.T.);
#1205=ORIENTED_EDGE('',*,*,#2195,.T.);
#1206=ORIENTED_EDGE('',*,*,#2196,.T.);
#1207=ORIENTED_EDGE('',*,*,#2192,.F.);
#1208=ORIENTED_EDGE('',*,*,#2197,.T.);
#1209=ORIENTED_EDGE('',*,*,#2185,.T.);
#1210=ORIENTED_EDGE('',*,*,#2198,.T.);
#1211=ORIENTED_EDGE('',*,*,#2199,.T.);
#1212=ORIENTED_EDGE('',*,*,#2200,.T.);
#1213=ORIENTED_EDGE('',*,*,#2201,.T.);
#1214=ORIENTED_EDGE('',*,*,#2202,.T.);
#1215=ORIENTED_EDGE('',*,*,#2203,.T.);
#1216=ORIENTED_EDGE('',*,*,#2204,.T.);
#1217=ORIENTED_EDGE('',*,*,#2205,.F.);
#1218=ORIENTED_EDGE('',*,*,#2206,.T.);
#1219=ORIENTED_EDGE('',*,*,#2207,.T.);
#1220=ORIENTED_EDGE('',*,*,#2085,.F.);
#1221=ORIENTED_EDGE('',*,*,#2208,.T.);
#1222=ORIENTED_EDGE('',*,*,#2209,.F.);
#1223=ORIENTED_EDGE('',*,*,#2210,.T.);
#1224=ORIENTED_EDGE('',*,*,#2205,.T.);
#1225=ORIENTED_EDGE('',*,*,#2211,.T.);
#1226=ORIENTED_EDGE('',*,*,#2212,.T.);
#1227=ORIENTED_EDGE('',*,*,#2213,.T.);
#1228=ORIENTED_EDGE('',*,*,#2209,.T.);
#1229=ORIENTED_EDGE('',*,*,#2214,.T.);
#1230=ORIENTED_EDGE('',*,*,#2135,.F.);
#1231=ORIENTED_EDGE('',*,*,#2215,.F.);
#1232=ORIENTED_EDGE('',*,*,#2216,.T.);
#1233=ORIENTED_EDGE('',*,*,#2217,.T.);
#1234=ORIENTED_EDGE('',*,*,#2077,.F.);
#1235=ORIENTED_EDGE('',*,*,#2218,.T.);
#1236=ORIENTED_EDGE('',*,*,#2219,.F.);
#1237=ORIENTED_EDGE('',*,*,#2220,.T.);
#1238=ORIENTED_EDGE('',*,*,#2215,.T.);
#1239=ORIENTED_EDGE('',*,*,#2221,.T.);
#1240=ORIENTED_EDGE('',*,*,#2222,.T.);
#1241=ORIENTED_EDGE('',*,*,#2223,.T.);
#1242=ORIENTED_EDGE('',*,*,#2219,.T.);
#1243=ORIENTED_EDGE('',*,*,#2224,.T.);
#1244=ORIENTED_EDGE('',*,*,#2127,.F.);
#1245=ORIENTED_EDGE('',*,*,#2225,.T.);
#1246=ORIENTED_EDGE('',*,*,#2226,.T.);
#1247=ORIENTED_EDGE('',*,*,#2227,.T.);
#1248=ORIENTED_EDGE('',*,*,#2131,.F.);
#1249=ORIENTED_EDGE('',*,*,#2228,.T.);
#1250=ORIENTED_EDGE('',*,*,#2089,.F.);
#1251=ORIENTED_EDGE('',*,*,#2229,.T.);
#1252=ORIENTED_EDGE('',*,*,#2230,.T.);
#1253=ORIENTED_EDGE('',*,*,#2231,.T.);
#1254=ORIENTED_EDGE('',*,*,#2123,.F.);
#1255=ORIENTED_EDGE('',*,*,#2232,.T.);
#1256=ORIENTED_EDGE('',*,*,#2081,.F.);
#1257=ORIENTED_EDGE('',*,*,#2233,.F.);
#1258=ORIENTED_EDGE('',*,*,#2178,.F.);
#1259=ORIENTED_EDGE('',*,*,#2234,.F.);
#1260=ORIENTED_EDGE('',*,*,#2182,.F.);
#1261=ORIENTED_EDGE('',*,*,#2234,.T.);
#1262=ORIENTED_EDGE('',*,*,#2174,.F.);
#1263=ORIENTED_EDGE('',*,*,#2235,.F.);
#1264=ORIENTED_EDGE('',*,*,#2179,.F.);
#1265=ORIENTED_EDGE('',*,*,#2233,.T.);
#1266=ORIENTED_EDGE('',*,*,#2181,.F.);
#1267=ORIENTED_EDGE('',*,*,#2236,.F.);
#1268=ORIENTED_EDGE('',*,*,#2164,.F.);
#1269=ORIENTED_EDGE('',*,*,#2235,.T.);
#1270=ORIENTED_EDGE('',*,*,#2167,.F.);
#1271=ORIENTED_EDGE('',*,*,#2236,.T.);
#1272=ORIENTED_EDGE('',*,*,#2180,.F.);
#1273=ORIENTED_EDGE('',*,*,#2237,.T.);
#1274=ORIENTED_EDGE('',*,*,#2238,.T.);
#1275=ORIENTED_EDGE('',*,*,#2239,.T.);
#1276=ORIENTED_EDGE('',*,*,#2240,.F.);
#1277=ORIENTED_EDGE('',*,*,#2241,.F.);
#1278=ORIENTED_EDGE('',*,*,#2130,.F.);
#1279=ORIENTED_EDGE('',*,*,#2242,.F.);
#1280=ORIENTED_EDGE('',*,*,#2190,.F.);
#1281=ORIENTED_EDGE('',*,*,#2242,.T.);
#1282=ORIENTED_EDGE('',*,*,#2129,.F.);
#1283=ORIENTED_EDGE('',*,*,#2243,.F.);
#1284=ORIENTED_EDGE('',*,*,#2184,.F.);
#1285=ORIENTED_EDGE('',*,*,#2241,.T.);
#1286=ORIENTED_EDGE('',*,*,#2189,.F.);
#1287=ORIENTED_EDGE('',*,*,#2244,.F.);
#1288=ORIENTED_EDGE('',*,*,#2228,.F.);
#1289=ORIENTED_EDGE('',*,*,#2243,.T.);
#1290=ORIENTED_EDGE('',*,*,#2136,.F.);
#1291=ORIENTED_EDGE('',*,*,#2245,.F.);
#1292=ORIENTED_EDGE('',*,*,#2198,.F.);
#1293=ORIENTED_EDGE('',*,*,#2244,.T.);
#1294=ORIENTED_EDGE('',*,*,#2188,.F.);
#1295=ORIENTED_EDGE('',*,*,#2246,.F.);
#1296=ORIENTED_EDGE('',*,*,#2090,.F.);
#1297=ORIENTED_EDGE('',*,*,#2214,.F.);
#1298=ORIENTED_EDGE('',*,*,#2247,.F.);
#1299=ORIENTED_EDGE('',*,*,#2199,.F.);
#1300=ORIENTED_EDGE('',*,*,#2245,.T.);
#1301=ORIENTED_EDGE('',*,*,#2246,.T.);
#1302=ORIENTED_EDGE('',*,*,#2193,.F.);
#1303=ORIENTED_EDGE('',*,*,#2248,.F.);
#1304=ORIENTED_EDGE('',*,*,#2083,.F.);
#1305=ORIENTED_EDGE('',*,*,#2247,.T.);
#1306=ORIENTED_EDGE('',*,*,#2211,.F.);
#1307=ORIENTED_EDGE('',*,*,#2249,.F.);
#1308=ORIENTED_EDGE('',*,*,#2200,.F.);
#1309=ORIENTED_EDGE('',*,*,#2248,.T.);
#1310=ORIENTED_EDGE('',*,*,#2196,.F.);
#1311=ORIENTED_EDGE('',*,*,#2250,.F.);
#1312=ORIENTED_EDGE('',*,*,#2084,.F.);
#1313=ORIENTED_EDGE('',*,*,#2249,.T.);
#1314=ORIENTED_EDGE('',*,*,#2208,.F.);
#1315=ORIENTED_EDGE('',*,*,#2250,.T.);
#1316=ORIENTED_EDGE('',*,*,#2195,.F.);
#1317=ORIENTED_EDGE('',*,*,#2137,.F.);
#1318=ORIENTED_EDGE('',*,*,#2251,.T.);
#1319=ORIENTED_EDGE('',*,*,#2024,.F.);
#1320=ORIENTED_EDGE('',*,*,#2252,.T.);
#1321=ORIENTED_EDGE('',*,*,#2227,.F.);
#1322=ORIENTED_EDGE('',*,*,#2253,.T.);
#1323=ORIENTED_EDGE('',*,*,#2144,.F.);
#1324=ORIENTED_EDGE('',*,*,#2254,.F.);
#1325=ORIENTED_EDGE('',*,*,#2254,.T.);
#1326=ORIENTED_EDGE('',*,*,#2143,.F.);
#1327=ORIENTED_EDGE('',*,*,#2255,.F.);
#1328=ORIENTED_EDGE('',*,*,#2132,.F.);
#1329=ORIENTED_EDGE('',*,*,#2255,.T.);
#1330=ORIENTED_EDGE('',*,*,#2157,.F.);
#1331=ORIENTED_EDGE('',*,*,#2256,.F.);
#1332=ORIENTED_EDGE('',*,*,#2133,.F.);
#1333=ORIENTED_EDGE('',*,*,#2256,.T.);
#1334=ORIENTED_EDGE('',*,*,#2101,.F.);
#1335=ORIENTED_EDGE('',*,*,#2257,.F.);
#1336=ORIENTED_EDGE('',*,*,#2134,.F.);
#1337=ORIENTED_EDGE('',*,*,#2100,.F.);
#1338=ORIENTED_EDGE('',*,*,#2258,.T.);
#1339=ORIENTED_EDGE('',*,*,#2212,.F.);
#1340=ORIENTED_EDGE('',*,*,#2257,.T.);
#1341=ORIENTED_EDGE('',*,*,#2149,.F.);
#1342=ORIENTED_EDGE('',*,*,#2259,.T.);
#1343=ORIENTED_EDGE('',*,*,#2026,.F.);
#1344=ORIENTED_EDGE('',*,*,#2260,.T.);
#1345=ORIENTED_EDGE('',*,*,#2150,.F.);
#1346=ORIENTED_EDGE('',*,*,#2261,.T.);
#1347=ORIENTED_EDGE('',*,*,#2225,.F.);
#1348=ORIENTED_EDGE('',*,*,#2262,.F.);
#1349=ORIENTED_EDGE('',*,*,#2262,.T.);
#1350=ORIENTED_EDGE('',*,*,#2088,.F.);
#1351=ORIENTED_EDGE('',*,*,#2263,.F.);
#1352=ORIENTED_EDGE('',*,*,#2151,.F.);
#1353=ORIENTED_EDGE('',*,*,#2263,.T.);
#1354=ORIENTED_EDGE('',*,*,#2087,.F.);
#1355=ORIENTED_EDGE('',*,*,#2264,.F.);
#1356=ORIENTED_EDGE('',*,*,#2155,.F.);
#1357=ORIENTED_EDGE('',*,*,#2264,.T.);
#1358=ORIENTED_EDGE('',*,*,#2086,.F.);
#1359=ORIENTED_EDGE('',*,*,#2265,.F.);
#1360=ORIENTED_EDGE('',*,*,#2113,.F.);
#1361=ORIENTED_EDGE('',*,*,#2207,.F.);
#1362=ORIENTED_EDGE('',*,*,#2266,.T.);
#1363=ORIENTED_EDGE('',*,*,#2106,.F.);
#1364=ORIENTED_EDGE('',*,*,#2265,.T.);
#1365=ORIENTED_EDGE('',*,*,#2267,.F.);
#1366=ORIENTED_EDGE('',*,*,#2122,.F.);
#1367=ORIENTED_EDGE('',*,*,#2268,.F.);
#1368=ORIENTED_EDGE('',*,*,#2177,.F.);
#1369=ORIENTED_EDGE('',*,*,#2268,.T.);
#1370=ORIENTED_EDGE('',*,*,#2121,.F.);
#1371=ORIENTED_EDGE('',*,*,#2269,.F.);
#1372=ORIENTED_EDGE('',*,*,#2173,.F.);
#1373=ORIENTED_EDGE('',*,*,#2267,.T.);
#1374=ORIENTED_EDGE('',*,*,#2176,.F.);
#1375=ORIENTED_EDGE('',*,*,#2270,.F.);
#1376=ORIENTED_EDGE('',*,*,#2232,.F.);
#1377=ORIENTED_EDGE('',*,*,#2269,.T.);
#1378=ORIENTED_EDGE('',*,*,#2128,.F.);
#1379=ORIENTED_EDGE('',*,*,#2271,.F.);
#1380=ORIENTED_EDGE('',*,*,#2169,.F.);
#1381=ORIENTED_EDGE('',*,*,#2270,.T.);
#1382=ORIENTED_EDGE('',*,*,#2175,.F.);
#1383=ORIENTED_EDGE('',*,*,#2272,.F.);
#1384=ORIENTED_EDGE('',*,*,#2082,.F.);
#1385=ORIENTED_EDGE('',*,*,#2224,.F.);
#1386=ORIENTED_EDGE('',*,*,#2273,.F.);
#1387=ORIENTED_EDGE('',*,*,#2170,.F.);
#1388=ORIENTED_EDGE('',*,*,#2271,.T.);
#1389=ORIENTED_EDGE('',*,*,#2272,.T.);
#1390=ORIENTED_EDGE('',*,*,#2162,.F.);
#1391=ORIENTED_EDGE('',*,*,#2274,.F.);
#1392=ORIENTED_EDGE('',*,*,#2075,.F.);
#1393=ORIENTED_EDGE('',*,*,#2273,.T.);
#1394=ORIENTED_EDGE('',*,*,#2221,.F.);
#1395=ORIENTED_EDGE('',*,*,#2275,.F.);
#1396=ORIENTED_EDGE('',*,*,#2171,.F.);
#1397=ORIENTED_EDGE('',*,*,#2274,.T.);
#1398=ORIENTED_EDGE('',*,*,#2166,.F.);
#1399=ORIENTED_EDGE('',*,*,#2276,.F.);
#1400=ORIENTED_EDGE('',*,*,#2076,.F.);
#1401=ORIENTED_EDGE('',*,*,#2275,.T.);
#1402=ORIENTED_EDGE('',*,*,#2218,.F.);
#1403=ORIENTED_EDGE('',*,*,#2276,.T.);
#1404=ORIENTED_EDGE('',*,*,#2165,.F.);
#1405=ORIENTED_EDGE('',*,*,#2147,.F.);
#1406=ORIENTED_EDGE('',*,*,#2277,.T.);
#1407=ORIENTED_EDGE('',*,*,#2029,.F.);
#1408=ORIENTED_EDGE('',*,*,#2278,.T.);
#1409=ORIENTED_EDGE('',*,*,#2231,.F.);
#1410=ORIENTED_EDGE('',*,*,#2279,.T.);
#1411=ORIENTED_EDGE('',*,*,#2154,.F.);
#1412=ORIENTED_EDGE('',*,*,#2280,.F.);
#1413=ORIENTED_EDGE('',*,*,#2280,.T.);
#1414=ORIENTED_EDGE('',*,*,#2153,.F.);
#1415=ORIENTED_EDGE('',*,*,#2281,.F.);
#1416=ORIENTED_EDGE('',*,*,#2124,.F.);
#1417=ORIENTED_EDGE('',*,*,#2281,.T.);
#1418=ORIENTED_EDGE('',*,*,#2156,.F.);
#1419=ORIENTED_EDGE('',*,*,#2282,.F.);
#1420=ORIENTED_EDGE('',*,*,#2125,.F.);
#1421=ORIENTED_EDGE('',*,*,#2282,.T.);
#1422=ORIENTED_EDGE('',*,*,#2111,.F.);
#1423=ORIENTED_EDGE('',*,*,#2283,.F.);
#1424=ORIENTED_EDGE('',*,*,#2126,.F.);
#1425=ORIENTED_EDGE('',*,*,#2110,.F.);
#1426=ORIENTED_EDGE('',*,*,#2284,.T.);
#1427=ORIENTED_EDGE('',*,*,#2222,.F.);
#1428=ORIENTED_EDGE('',*,*,#2283,.T.);
#1429=ORIENTED_EDGE('',*,*,#2031,.F.);
#1430=ORIENTED_EDGE('',*,*,#2285,.T.);
#1431=ORIENTED_EDGE('',*,*,#2139,.F.);
#1432=ORIENTED_EDGE('',*,*,#2286,.T.);
#1433=ORIENTED_EDGE('',*,*,#2140,.F.);
#1434=ORIENTED_EDGE('',*,*,#2287,.T.);
#1435=ORIENTED_EDGE('',*,*,#2229,.F.);
#1436=ORIENTED_EDGE('',*,*,#2288,.F.);
#1437=ORIENTED_EDGE('',*,*,#2288,.T.);
#1438=ORIENTED_EDGE('',*,*,#2080,.F.);
#1439=ORIENTED_EDGE('',*,*,#2289,.F.);
#1440=ORIENTED_EDGE('',*,*,#2141,.F.);
#1441=ORIENTED_EDGE('',*,*,#2289,.T.);
#1442=ORIENTED_EDGE('',*,*,#2079,.F.);
#1443=ORIENTED_EDGE('',*,*,#2290,.F.);
#1444=ORIENTED_EDGE('',*,*,#2158,.F.);
#1445=ORIENTED_EDGE('',*,*,#2290,.T.);
#1446=ORIENTED_EDGE('',*,*,#2078,.F.);
#1447=ORIENTED_EDGE('',*,*,#2291,.F.);
#1448=ORIENTED_EDGE('',*,*,#2103,.F.);
#1449=ORIENTED_EDGE('',*,*,#2217,.F.);
#1450=ORIENTED_EDGE('',*,*,#2292,.T.);
#1451=ORIENTED_EDGE('',*,*,#2104,.F.);
#1452=ORIENTED_EDGE('',*,*,#2291,.T.);
#1453=ORIENTED_EDGE('',*,*,#2293,.F.);
#1454=ORIENTED_EDGE('',*,*,#2204,.F.);
#1455=ORIENTED_EDGE('',*,*,#2294,.F.);
#1456=ORIENTED_EDGE('',*,*,#2197,.F.);
#1457=ORIENTED_EDGE('',*,*,#2294,.T.);
#1458=ORIENTED_EDGE('',*,*,#2203,.F.);
#1459=ORIENTED_EDGE('',*,*,#2295,.F.);
#1460=ORIENTED_EDGE('',*,*,#2186,.F.);
#1461=ORIENTED_EDGE('',*,*,#2293,.T.);
#1462=ORIENTED_EDGE('',*,*,#2194,.F.);
#1463=ORIENTED_EDGE('',*,*,#2296,.F.);
#1464=ORIENTED_EDGE('',*,*,#2201,.F.);
#1465=ORIENTED_EDGE('',*,*,#2295,.T.);
#1466=ORIENTED_EDGE('',*,*,#2202,.F.);
#1467=ORIENTED_EDGE('',*,*,#2296,.T.);
#1468=ORIENTED_EDGE('',*,*,#2191,.F.);
#1469=ORIENTED_EDGE('',*,*,#2297,.F.);
#1470=ORIENTED_EDGE('',*,*,#2287,.F.);
#1471=ORIENTED_EDGE('',*,*,#2285,.F.);
#1472=ORIENTED_EDGE('',*,*,#2298,.F.);
#1473=ORIENTED_EDGE('',*,*,#2230,.F.);
#1474=ORIENTED_EDGE('',*,*,#2297,.T.);
#1475=ORIENTED_EDGE('',*,*,#2030,.F.);
#1476=ORIENTED_EDGE('',*,*,#2298,.T.);
#1477=ORIENTED_EDGE('',*,*,#2277,.F.);
#1478=ORIENTED_EDGE('',*,*,#2279,.F.);
#1479=ORIENTED_EDGE('',*,*,#2299,.F.);
#1480=ORIENTED_EDGE('',*,*,#2252,.F.);
#1481=ORIENTED_EDGE('',*,*,#2064,.F.);
#1482=ORIENTED_EDGE('',*,*,#2299,.T.);
#1483=ORIENTED_EDGE('',*,*,#2042,.F.);
#1484=ORIENTED_EDGE('',*,*,#2300,.F.);
#1485=ORIENTED_EDGE('',*,*,#2138,.F.);
#1486=ORIENTED_EDGE('',*,*,#2286,.F.);
#1487=ORIENTED_EDGE('',*,*,#2300,.T.);
#1488=ORIENTED_EDGE('',*,*,#2066,.F.);
#1489=ORIENTED_EDGE('',*,*,#2068,.T.);
#1490=ORIENTED_EDGE('',*,*,#2259,.F.);
#1491=ORIENTED_EDGE('',*,*,#2301,.F.);
#1492=ORIENTED_EDGE('',*,*,#2301,.T.);
#1493=ORIENTED_EDGE('',*,*,#2148,.F.);
#1494=ORIENTED_EDGE('',*,*,#2302,.F.);
#1495=ORIENTED_EDGE('',*,*,#2037,.F.);
#1496=ORIENTED_EDGE('',*,*,#2302,.T.);
#1497=ORIENTED_EDGE('',*,*,#2278,.F.);
#1498=ORIENTED_EDGE('',*,*,#2070,.T.);
#1499=ORIENTED_EDGE('',*,*,#2303,.F.);
#1500=ORIENTED_EDGE('',*,*,#2261,.F.);
#1501=ORIENTED_EDGE('',*,*,#2260,.F.);
#1502=ORIENTED_EDGE('',*,*,#2304,.F.);
#1503=ORIENTED_EDGE('',*,*,#2226,.F.);
#1504=ORIENTED_EDGE('',*,*,#2303,.T.);
#1505=ORIENTED_EDGE('',*,*,#2025,.F.);
#1506=ORIENTED_EDGE('',*,*,#2304,.T.);
#1507=ORIENTED_EDGE('',*,*,#2251,.F.);
#1508=ORIENTED_EDGE('',*,*,#2253,.F.);
#1509=ORIENTED_EDGE('',*,*,#2305,.F.);
#1510=ORIENTED_EDGE('',*,*,#2145,.F.);
#1511=ORIENTED_EDGE('',*,*,#2306,.F.);
#1512=ORIENTED_EDGE('',*,*,#2096,.F.);
#1513=ORIENTED_EDGE('',*,*,#2306,.T.);
#1514=ORIENTED_EDGE('',*,*,#2107,.F.);
#1515=ORIENTED_EDGE('',*,*,#2307,.F.);
#1516=ORIENTED_EDGE('',*,*,#2091,.F.);
#1517=ORIENTED_EDGE('',*,*,#2305,.T.);
#1518=ORIENTED_EDGE('',*,*,#2095,.F.);
#1519=ORIENTED_EDGE('',*,*,#2308,.F.);
#1520=ORIENTED_EDGE('',*,*,#2099,.F.);
#1521=ORIENTED_EDGE('',*,*,#2307,.T.);
#1522=ORIENTED_EDGE('',*,*,#2266,.F.);
#1523=ORIENTED_EDGE('',*,*,#2309,.F.);
#1524=ORIENTED_EDGE('',*,*,#2258,.F.);
#1525=ORIENTED_EDGE('',*,*,#2308,.T.);
#1526=ORIENTED_EDGE('',*,*,#2310,.F.);
#1527=ORIENTED_EDGE('',*,*,#2309,.T.);
#1528=ORIENTED_EDGE('',*,*,#2206,.F.);
#1529=ORIENTED_EDGE('',*,*,#2311,.F.);
#1530=ORIENTED_EDGE('',*,*,#2092,.F.);
#1531=ORIENTED_EDGE('',*,*,#2310,.T.);
#1532=ORIENTED_EDGE('',*,*,#2094,.F.);
#1533=ORIENTED_EDGE('',*,*,#2312,.F.);
#1534=ORIENTED_EDGE('',*,*,#2213,.F.);
#1535=ORIENTED_EDGE('',*,*,#2311,.T.);
#1536=ORIENTED_EDGE('',*,*,#2210,.F.);
#1537=ORIENTED_EDGE('',*,*,#2312,.T.);
#1538=ORIENTED_EDGE('',*,*,#2093,.F.);
#1539=ORIENTED_EDGE('',*,*,#2097,.F.);
#1540=ORIENTED_EDGE('',*,*,#2240,.T.);
#1541=ORIENTED_EDGE('',*,*,#2159,.F.);
#1542=ORIENTED_EDGE('',*,*,#2239,.F.);
#1543=ORIENTED_EDGE('',*,*,#2237,.F.);
#1544=ORIENTED_EDGE('',*,*,#2160,.F.);
#1545=ORIENTED_EDGE('',*,*,#2313,.F.);
#1546=ORIENTED_EDGE('',*,*,#2119,.F.);
#1547=ORIENTED_EDGE('',*,*,#2314,.F.);
#1548=ORIENTED_EDGE('',*,*,#2146,.F.);
#1549=ORIENTED_EDGE('',*,*,#2314,.T.);
#1550=ORIENTED_EDGE('',*,*,#2118,.F.);
#1551=ORIENTED_EDGE('',*,*,#2315,.F.);
#1552=ORIENTED_EDGE('',*,*,#2109,.F.);
#1553=ORIENTED_EDGE('',*,*,#2313,.T.);
#1554=ORIENTED_EDGE('',*,*,#2105,.F.);
#1555=ORIENTED_EDGE('',*,*,#2316,.F.);
#1556=ORIENTED_EDGE('',*,*,#2114,.F.);
#1557=ORIENTED_EDGE('',*,*,#2284,.F.);
#1558=ORIENTED_EDGE('',*,*,#2315,.T.);
#1559=ORIENTED_EDGE('',*,*,#2317,.F.);
#1560=ORIENTED_EDGE('',*,*,#2316,.T.);
#1561=ORIENTED_EDGE('',*,*,#2292,.F.);
#1562=ORIENTED_EDGE('',*,*,#2318,.F.);
#1563=ORIENTED_EDGE('',*,*,#2317,.T.);
#1564=ORIENTED_EDGE('',*,*,#2117,.F.);
#1565=ORIENTED_EDGE('',*,*,#2319,.F.);
#1566=ORIENTED_EDGE('',*,*,#2223,.F.);
#1567=ORIENTED_EDGE('',*,*,#2318,.T.);
#1568=ORIENTED_EDGE('',*,*,#2216,.F.);
#1569=ORIENTED_EDGE('',*,*,#2320,.F.);
#1570=ORIENTED_EDGE('',*,*,#2115,.F.);
#1571=ORIENTED_EDGE('',*,*,#2319,.T.);
#1572=ORIENTED_EDGE('',*,*,#2116,.F.);
#1573=ORIENTED_EDGE('',*,*,#2320,.T.);
#1574=ORIENTED_EDGE('',*,*,#2220,.F.);
#1575=ORIENTED_EDGE('',*,*,#2120,.F.);
#1576=ORIENTED_EDGE('',*,*,#2238,.F.);
#1577=ORIENTED_EDGE('',*,*,#2027,.T.);
#1578=ORIENTED_EDGE('',*,*,#2072,.T.);
#1579=ORIENTED_EDGE('',*,*,#2053,.T.);
#1580=ORIENTED_EDGE('',*,*,#2056,.F.);
#1581=ORIENTED_EDGE('',*,*,#2043,.T.);
#1582=ORIENTED_EDGE('',*,*,#2061,.F.);
#1583=ORIENTED_EDGE('',*,*,#2058,.F.);
#1584=ORIENTED_EDGE('',*,*,#2074,.T.);
#1585=ORIENTED_EDGE('',*,*,#2020,.F.);
#1586=ORIENTED_EDGE('',*,*,#2067,.F.);
#1587=ORIENTED_EDGE('',*,*,#2035,.T.);
#1588=ORIENTED_EDGE('',*,*,#2069,.F.);
#1589=ORIENTED_EDGE('',*,*,#2048,.T.);
#1590=ORIENTED_EDGE('',*,*,#2051,.T.);
#1591=ORIENTED_EDGE('',*,*,#2071,.T.);
#1592=ORIENTED_EDGE('',*,*,#2033,.T.);
#1593=ORIENTED_EDGE('',*,*,#2065,.F.);
#1594=ORIENTED_EDGE('',*,*,#2040,.F.);
#1595=ORIENTED_EDGE('',*,*,#2063,.F.);
#1596=ORIENTED_EDGE('',*,*,#2022,.F.);
#1597=ORIENTED_EDGE('',*,*,#2073,.T.);
#1598=ORIENTED_EDGE('',*,*,#2060,.F.);
#1599=ORIENTED_EDGE('',*,*,#2062,.F.);
#1600=ORIENTED_EDGE('',*,*,#2045,.T.);
#1601=ORIENTED_EDGE('',*,*,#2055,.F.);
#1602=ORIENTED_EDGE('',*,*,#2050,.T.);
#1603=ORIENTED_EDGE('',*,*,#2321,.F.);
#1604=ORIENTED_EDGE('',*,*,#2322,.F.);
#1605=ORIENTED_EDGE('',*,*,#2323,.T.);
#1606=ORIENTED_EDGE('',*,*,#2324,.F.);
#1607=ORIENTED_EDGE('',*,*,#2325,.T.);
#1608=ORIENTED_EDGE('',*,*,#2321,.T.);
#1609=ORIENTED_EDGE('',*,*,#2326,.T.);
#1610=ORIENTED_EDGE('',*,*,#2327,.T.);
#1611=ORIENTED_EDGE('',*,*,#2323,.F.);
#1612=ORIENTED_EDGE('',*,*,#2328,.F.);
#1613=ORIENTED_EDGE('',*,*,#2329,.F.);
#1614=ORIENTED_EDGE('',*,*,#2330,.F.);
#1615=ORIENTED_EDGE('',*,*,#2330,.T.);
#1616=ORIENTED_EDGE('',*,*,#2331,.T.);
#1617=ORIENTED_EDGE('',*,*,#2326,.F.);
#1618=ORIENTED_EDGE('',*,*,#2324,.T.);
#1619=ORIENTED_EDGE('',*,*,#2328,.T.);
#1620=ORIENTED_EDGE('',*,*,#2322,.T.);
#1621=ORIENTED_EDGE('',*,*,#2325,.F.);
#1622=ORIENTED_EDGE('',*,*,#2332,.T.);
#1623=ORIENTED_EDGE('',*,*,#2327,.F.);
#1624=ORIENTED_EDGE('',*,*,#2331,.F.);
#1625=ORIENTED_EDGE('',*,*,#2329,.T.);
#1626=ORIENTED_EDGE('',*,*,#2332,.F.);
#1627=ORIENTED_EDGE('',*,*,#2333,.T.);
#1628=ORIENTED_EDGE('',*,*,#2334,.F.);
#1629=ORIENTED_EDGE('',*,*,#2335,.F.);
#1630=ORIENTED_EDGE('',*,*,#2336,.T.);
#1631=ORIENTED_EDGE('',*,*,#2333,.F.);
#1632=ORIENTED_EDGE('',*,*,#2335,.T.);
#1633=ORIENTED_EDGE('',*,*,#2334,.T.);
#1634=ORIENTED_EDGE('',*,*,#2336,.F.);
#1635=ORIENTED_EDGE('',*,*,#2337,.T.);
#1636=ORIENTED_EDGE('',*,*,#2338,.F.);
#1637=ORIENTED_EDGE('',*,*,#2339,.T.);
#1638=ORIENTED_EDGE('',*,*,#2340,.T.);
#1639=ORIENTED_EDGE('',*,*,#2341,.F.);
#1640=ORIENTED_EDGE('',*,*,#2342,.T.);
#1641=ORIENTED_EDGE('',*,*,#2343,.F.);
#1642=ORIENTED_EDGE('',*,*,#2344,.T.);
#1643=ORIENTED_EDGE('',*,*,#2345,.F.);
#1644=ORIENTED_EDGE('',*,*,#2346,.F.);
#1645=ORIENTED_EDGE('',*,*,#2347,.F.);
#1646=ORIENTED_EDGE('',*,*,#2348,.F.);
#1647=ORIENTED_EDGE('',*,*,#2349,.F.);
#1648=ORIENTED_EDGE('',*,*,#2345,.T.);
#1649=ORIENTED_EDGE('',*,*,#2350,.F.);
#1650=ORIENTED_EDGE('',*,*,#2351,.F.);
#1651=ORIENTED_EDGE('',*,*,#2352,.T.);
#1652=ORIENTED_EDGE('',*,*,#2340,.F.);
#1653=ORIENTED_EDGE('',*,*,#2353,.T.);
#1654=ORIENTED_EDGE('',*,*,#2354,.F.);
#1655=ORIENTED_EDGE('',*,*,#2346,.T.);
#1656=ORIENTED_EDGE('',*,*,#2355,.T.);
#1657=ORIENTED_EDGE('',*,*,#2356,.T.);
#1658=ORIENTED_EDGE('',*,*,#2357,.T.);
#1659=ORIENTED_EDGE('',*,*,#2358,.F.);
#1660=ORIENTED_EDGE('',*,*,#2347,.T.);
#1661=ORIENTED_EDGE('',*,*,#2354,.T.);
#1662=ORIENTED_EDGE('',*,*,#2359,.F.);
#1663=ORIENTED_EDGE('',*,*,#2360,.T.);
#1664=ORIENTED_EDGE('',*,*,#2361,.T.);
#1665=ORIENTED_EDGE('',*,*,#2362,.T.);
#1666=ORIENTED_EDGE('',*,*,#2363,.F.);
#1667=ORIENTED_EDGE('',*,*,#2364,.F.);
#1668=ORIENTED_EDGE('',*,*,#2348,.T.);
#1669=ORIENTED_EDGE('',*,*,#2358,.T.);
#1670=ORIENTED_EDGE('',*,*,#2365,.T.);
#1671=ORIENTED_EDGE('',*,*,#2342,.F.);
#1672=ORIENTED_EDGE('',*,*,#2350,.T.);
#1673=ORIENTED_EDGE('',*,*,#2349,.T.);
#1674=ORIENTED_EDGE('',*,*,#2364,.T.);
#1675=ORIENTED_EDGE('',*,*,#2366,.F.);
#1676=ORIENTED_EDGE('',*,*,#2355,.F.);
#1677=ORIENTED_EDGE('',*,*,#2367,.T.);
#1678=ORIENTED_EDGE('',*,*,#2368,.T.);
#1679=ORIENTED_EDGE('',*,*,#2369,.T.);
#1680=ORIENTED_EDGE('',*,*,#2370,.F.);
#1681=ORIENTED_EDGE('',*,*,#2363,.T.);
#1682=ORIENTED_EDGE('',*,*,#2371,.F.);
#1683=ORIENTED_EDGE('',*,*,#2356,.F.);
#1684=ORIENTED_EDGE('',*,*,#2366,.T.);
#1685=ORIENTED_EDGE('',*,*,#2362,.F.);
#1686=ORIENTED_EDGE('',*,*,#2372,.T.);
#1687=ORIENTED_EDGE('',*,*,#2373,.F.);
#1688=ORIENTED_EDGE('',*,*,#2374,.T.);
#1689=ORIENTED_EDGE('',*,*,#2357,.F.);
#1690=ORIENTED_EDGE('',*,*,#2371,.T.);
#1691=ORIENTED_EDGE('',*,*,#2375,.F.);
#1692=ORIENTED_EDGE('',*,*,#2351,.T.);
#1693=ORIENTED_EDGE('',*,*,#2374,.F.);
#1694=ORIENTED_EDGE('',*,*,#2376,.F.);
#1695=ORIENTED_EDGE('',*,*,#2352,.F.);
#1696=ORIENTED_EDGE('',*,*,#2375,.T.);
#1697=ORIENTED_EDGE('',*,*,#2377,.T.);
#1698=ORIENTED_EDGE('',*,*,#2378,.T.);
#1699=ORIENTED_EDGE('',*,*,#2360,.F.);
#1700=ORIENTED_EDGE('',*,*,#2341,.T.);
#1701=ORIENTED_EDGE('',*,*,#2365,.F.);
#1702=ORIENTED_EDGE('',*,*,#2359,.T.);
#1703=ORIENTED_EDGE('',*,*,#2353,.F.);
#1704=ORIENTED_EDGE('',*,*,#2343,.T.);
#1705=ORIENTED_EDGE('',*,*,#2378,.F.);
#1706=ORIENTED_EDGE('',*,*,#2379,.T.);
#1707=ORIENTED_EDGE('',*,*,#2372,.F.);
#1708=ORIENTED_EDGE('',*,*,#2361,.F.);
#1709=ORIENTED_EDGE('',*,*,#2380,.F.);
#1710=ORIENTED_EDGE('',*,*,#2367,.F.);
#1711=ORIENTED_EDGE('',*,*,#2381,.T.);
#1712=ORIENTED_EDGE('',*,*,#2382,.F.);
#1713=ORIENTED_EDGE('',*,*,#2368,.F.);
#1714=ORIENTED_EDGE('',*,*,#2380,.T.);
#1715=ORIENTED_EDGE('',*,*,#2383,.F.);
#1716=ORIENTED_EDGE('',*,*,#2384,.F.);
#1717=ORIENTED_EDGE('',*,*,#2377,.F.);
#1718=ORIENTED_EDGE('',*,*,#2376,.T.);
#1719=ORIENTED_EDGE('',*,*,#2373,.T.);
#1720=ORIENTED_EDGE('',*,*,#2379,.F.);
#1721=ORIENTED_EDGE('',*,*,#2385,.F.);
#1722=ORIENTED_EDGE('',*,*,#2339,.F.);
#1723=ORIENTED_EDGE('',*,*,#2386,.F.);
#1724=ORIENTED_EDGE('',*,*,#2387,.F.);
#1725=ORIENTED_EDGE('',*,*,#2388,.T.);
#1726=ORIENTED_EDGE('',*,*,#2382,.T.);
#1727=ORIENTED_EDGE('',*,*,#2389,.T.);
#1728=ORIENTED_EDGE('',*,*,#2390,.T.);
#1729=ORIENTED_EDGE('',*,*,#2391,.T.);
#1730=ORIENTED_EDGE('',*,*,#2392,.T.);
#1731=ORIENTED_EDGE('',*,*,#2393,.T.);
#1732=ORIENTED_EDGE('',*,*,#2394,.T.);
#1733=ORIENTED_EDGE('',*,*,#2395,.T.);
#1734=ORIENTED_EDGE('',*,*,#2391,.F.);
#1735=ORIENTED_EDGE('',*,*,#2396,.T.);
#1736=ORIENTED_EDGE('',*,*,#2393,.F.);
#1737=ORIENTED_EDGE('',*,*,#2389,.F.);
#1738=ORIENTED_EDGE('',*,*,#2381,.F.);
#1739=ORIENTED_EDGE('',*,*,#2388,.F.);
#1740=ORIENTED_EDGE('',*,*,#2397,.F.);
#1741=ORIENTED_EDGE('',*,*,#2398,.F.);
#1742=ORIENTED_EDGE('',*,*,#2399,.F.);
#1743=ORIENTED_EDGE('',*,*,#2400,.T.);
#1744=ORIENTED_EDGE('',*,*,#2384,.T.);
#1745=ORIENTED_EDGE('',*,*,#2401,.T.);
#1746=ORIENTED_EDGE('',*,*,#2402,.T.);
#1747=ORIENTED_EDGE('',*,*,#2403,.T.);
#1748=ORIENTED_EDGE('',*,*,#2403,.F.);
#1749=ORIENTED_EDGE('',*,*,#2404,.T.);
#1750=ORIENTED_EDGE('',*,*,#2401,.F.);
#1751=ORIENTED_EDGE('',*,*,#2383,.T.);
#1752=ORIENTED_EDGE('',*,*,#2400,.F.);
#1753=ORIENTED_EDGE('',*,*,#2399,.T.);
#1754=ORIENTED_EDGE('',*,*,#2385,.T.);
#1755=ORIENTED_EDGE('',*,*,#2405,.T.);
#1756=ORIENTED_EDGE('',*,*,#2406,.F.);
#1757=ORIENTED_EDGE('',*,*,#2407,.T.);
#1758=ORIENTED_EDGE('',*,*,#2408,.F.);
#1759=ORIENTED_EDGE('',*,*,#2337,.F.);
#1760=ORIENTED_EDGE('',*,*,#2409,.F.);
#1761=ORIENTED_EDGE('',*,*,#2387,.T.);
#1762=ORIENTED_EDGE('',*,*,#2410,.F.);
#1763=ORIENTED_EDGE('',*,*,#2397,.T.);
#1764=ORIENTED_EDGE('',*,*,#2390,.F.);
#1765=ORIENTED_EDGE('',*,*,#2392,.F.);
#1766=ORIENTED_EDGE('',*,*,#2395,.F.);
#1767=ORIENTED_EDGE('',*,*,#2411,.T.);
#1768=ORIENTED_EDGE('',*,*,#2396,.F.);
#1769=ORIENTED_EDGE('',*,*,#2394,.F.);
#1770=ORIENTED_EDGE('',*,*,#2402,.F.);
#1771=ORIENTED_EDGE('',*,*,#2404,.F.);
#1772=ORIENTED_EDGE('',*,*,#2412,.F.);
#1773=ORIENTED_EDGE('',*,*,#2413,.F.);
#1774=ORIENTED_EDGE('',*,*,#2414,.F.);
#1775=ORIENTED_EDGE('',*,*,#2415,.F.);
#1776=ORIENTED_EDGE('',*,*,#2416,.F.);
#1777=ORIENTED_EDGE('',*,*,#2417,.F.);
#1778=ORIENTED_EDGE('',*,*,#2418,.F.);
#1779=ORIENTED_EDGE('',*,*,#2405,.F.);
#1780=ORIENTED_EDGE('',*,*,#2419,.F.);
#1781=ORIENTED_EDGE('',*,*,#2420,.F.);
#1782=ORIENTED_EDGE('',*,*,#2406,.T.);
#1783=ORIENTED_EDGE('',*,*,#2418,.T.);
#1784=ORIENTED_EDGE('',*,*,#2421,.T.);
#1785=ORIENTED_EDGE('',*,*,#2407,.F.);
#1786=ORIENTED_EDGE('',*,*,#2420,.T.);
#1787=ORIENTED_EDGE('',*,*,#2422,.F.);
#1788=ORIENTED_EDGE('',*,*,#2423,.F.);
#1789=ORIENTED_EDGE('',*,*,#2424,.F.);
#1790=ORIENTED_EDGE('',*,*,#2425,.T.);
#1791=ORIENTED_EDGE('',*,*,#2426,.F.);
#1792=ORIENTED_EDGE('',*,*,#2427,.T.);
#1793=ORIENTED_EDGE('',*,*,#2428,.T.);
#1794=ORIENTED_EDGE('',*,*,#2409,.T.);
#1795=ORIENTED_EDGE('',*,*,#2408,.T.);
#1796=ORIENTED_EDGE('',*,*,#2428,.F.);
#1797=ORIENTED_EDGE('',*,*,#2429,.T.);
#1798=ORIENTED_EDGE('',*,*,#2419,.T.);
#1799=ORIENTED_EDGE('',*,*,#2430,.T.);
#1800=ORIENTED_EDGE('',*,*,#2410,.T.);
#1801=ORIENTED_EDGE('',*,*,#2427,.F.);
#1802=ORIENTED_EDGE('',*,*,#2431,.T.);
#1803=ORIENTED_EDGE('',*,*,#2412,.T.);
#1804=ORIENTED_EDGE('',*,*,#2429,.F.);
#1805=ORIENTED_EDGE('',*,*,#2426,.T.);
#1806=ORIENTED_EDGE('',*,*,#2432,.T.);
#1807=ORIENTED_EDGE('',*,*,#2433,.F.);
#1808=ORIENTED_EDGE('',*,*,#2434,.T.);
#1809=ORIENTED_EDGE('',*,*,#2413,.T.);
#1810=ORIENTED_EDGE('',*,*,#2431,.F.);
#1811=ORIENTED_EDGE('',*,*,#2435,.F.);
#1812=ORIENTED_EDGE('',*,*,#2436,.F.);
#1813=ORIENTED_EDGE('',*,*,#2414,.T.);
#1814=ORIENTED_EDGE('',*,*,#2434,.F.);
#1815=ORIENTED_EDGE('',*,*,#2424,.T.);
#1816=ORIENTED_EDGE('',*,*,#2437,.F.);
#1817=ORIENTED_EDGE('',*,*,#2415,.T.);
#1818=ORIENTED_EDGE('',*,*,#2436,.T.);
#1819=ORIENTED_EDGE('',*,*,#2438,.F.);
#1820=ORIENTED_EDGE('',*,*,#2439,.T.);
#1821=ORIENTED_EDGE('',*,*,#2430,.F.);
#1822=ORIENTED_EDGE('',*,*,#2416,.T.);
#1823=ORIENTED_EDGE('',*,*,#2437,.T.);
#1824=ORIENTED_EDGE('',*,*,#2423,.T.);
#1825=ORIENTED_EDGE('',*,*,#2440,.T.);
#1826=ORIENTED_EDGE('',*,*,#2417,.T.);
#1827=ORIENTED_EDGE('',*,*,#2440,.F.);
#1828=ORIENTED_EDGE('',*,*,#2422,.T.);
#1829=ORIENTED_EDGE('',*,*,#2421,.F.);
#1830=ORIENTED_EDGE('',*,*,#2425,.F.);
#1831=ORIENTED_EDGE('',*,*,#2439,.F.);
#1832=ORIENTED_EDGE('',*,*,#2441,.T.);
#1833=ORIENTED_EDGE('',*,*,#2432,.F.);
#1834=ORIENTED_EDGE('',*,*,#2438,.T.);
#1835=ORIENTED_EDGE('',*,*,#2435,.T.);
#1836=ORIENTED_EDGE('',*,*,#2433,.T.);
#1837=ORIENTED_EDGE('',*,*,#2441,.F.);
#1838=ORIENTED_EDGE('',*,*,#2386,.T.);
#1839=ORIENTED_EDGE('',*,*,#2411,.F.);
#1840=ORIENTED_EDGE('',*,*,#2398,.T.);
#1841=ORIENTED_EDGE('',*,*,#2369,.F.);
#1842=ORIENTED_EDGE('',*,*,#2338,.T.);
#1843=ORIENTED_EDGE('',*,*,#2370,.T.);
#1844=ORIENTED_EDGE('',*,*,#2344,.F.);
#1845=ORIENTED_EDGE('',*,*,#2442,.F.);
#1846=ORIENTED_EDGE('',*,*,#2443,.T.);
#1847=ORIENTED_EDGE('',*,*,#2444,.F.);
#1848=ORIENTED_EDGE('',*,*,#2445,.F.);
#1849=ORIENTED_EDGE('',*,*,#2446,.F.);
#1850=ORIENTED_EDGE('',*,*,#2447,.T.);
#1851=ORIENTED_EDGE('',*,*,#2448,.F.);
#1852=ORIENTED_EDGE('',*,*,#2445,.T.);
#1853=ORIENTED_EDGE('',*,*,#2449,.F.);
#1854=ORIENTED_EDGE('',*,*,#2450,.T.);
#1855=ORIENTED_EDGE('',*,*,#2443,.F.);
#1856=ORIENTED_EDGE('',*,*,#2451,.T.);
#1857=ORIENTED_EDGE('',*,*,#2452,.F.);
#1858=ORIENTED_EDGE('',*,*,#2449,.T.);
#1859=ORIENTED_EDGE('',*,*,#2453,.F.);
#1860=ORIENTED_EDGE('',*,*,#2447,.F.);
#1861=ORIENTED_EDGE('',*,*,#2448,.T.);
#1862=ORIENTED_EDGE('',*,*,#2453,.T.);
#1863=ORIENTED_EDGE('',*,*,#2451,.F.);
#1864=ORIENTED_EDGE('',*,*,#2442,.T.);
#1865=ORIENTED_EDGE('',*,*,#2446,.T.);
#1866=ORIENTED_EDGE('',*,*,#2444,.T.);
#1867=ORIENTED_EDGE('',*,*,#2450,.F.);
#1868=ORIENTED_EDGE('',*,*,#2452,.T.);
#1869=EDGE_CURVE('',#2454,#2455,#2834,.T.);
#1870=EDGE_CURVE('',#2454,#2456,#583,.T.);
#1871=EDGE_CURVE('',#2456,#2457,#584,.T.);
#1872=EDGE_CURVE('',#2457,#2458,#2835,.T.);
#1873=EDGE_CURVE('',#2455,#2458,#2836,.T.);
#1874=EDGE_CURVE('',#2459,#2460,#2837,.T.);
#1875=EDGE_CURVE('',#2459,#2461,#585,.T.);
#1876=EDGE_CURVE('',#2461,#2454,#586,.T.);
#1877=EDGE_CURVE('',#2460,#2455,#2838,.T.);
#1878=EDGE_CURVE('',#2462,#2463,#2839,.T.);
#1879=EDGE_CURVE('',#2462,#2464,#587,.F.);
#1880=EDGE_CURVE('',#2464,#2459,#588,.F.);
#1881=EDGE_CURVE('',#2463,#2460,#2840,.T.);
#1882=EDGE_CURVE('',#2465,#2466,#2841,.T.);
#1883=EDGE_CURVE('',#2465,#2467,#589,.T.);
#1884=EDGE_CURVE('',#2467,#2462,#590,.T.);
#1885=EDGE_CURVE('',#2466,#2463,#2842,.T.);
#1886=EDGE_CURVE('',#2468,#2469,#2843,.T.);
#1887=EDGE_CURVE('',#2468,#2470,#591,.T.);
#1888=EDGE_CURVE('',#2470,#2465,#592,.T.);
#1889=EDGE_CURVE('',#2469,#2466,#2844,.T.);
#1890=EDGE_CURVE('',#2457,#2471,#593,.T.);
#1891=EDGE_CURVE('',#2471,#2468,#594,.T.);
#1892=EDGE_CURVE('',#2458,#2469,#2845,.T.);
#1893=EDGE_CURVE('',#2472,#2472,#308,.T.);
#1894=EDGE_CURVE('',#2473,#2473,#309,.F.);
#1895=EDGE_CURVE('',#2474,#2474,#310,.F.);
#1896=EDGE_CURVE('',#2475,#2475,#311,.T.);
#1897=EDGE_CURVE('',#2470,#2471,#312,.T.);
#1898=EDGE_CURVE('',#2471,#2456,#313,.T.);
#1899=EDGE_CURVE('',#2467,#2470,#314,.T.);
#1900=EDGE_CURVE('',#2464,#2467,#315,.T.);
#1901=EDGE_CURVE('',#2461,#2464,#316,.T.);
#1902=EDGE_CURVE('',#2456,#2461,#317,.T.);
#1903=EDGE_CURVE('',#2476,#2476,#318,.T.);
#1904=EDGE_CURVE('',#2477,#2477,#319,.T.);
#1905=EDGE_CURVE('',#2478,#2478,#320,.T.);
#1906=EDGE_CURVE('',#2479,#2479,#321,.T.);
#1907=EDGE_CURVE('',#2480,#2481,#322,.T.);
#1908=EDGE_CURVE('',#2482,#2481,#2846,.T.);
#1909=EDGE_CURVE('',#2483,#2482,#323,.T.);
#1910=EDGE_CURVE('',#2483,#2480,#2847,.T.);
#1911=EDGE_CURVE('',#2481,#2484,#2848,.T.);
#1912=EDGE_CURVE('',#2485,#2484,#2849,.T.);
#1913=EDGE_CURVE('',#2482,#2485,#2850,.T.);
#1914=EDGE_CURVE('',#2484,#2486,#324,.T.);
#1915=EDGE_CURVE('',#2487,#2486,#2851,.T.);
#1916=EDGE_CURVE('',#2485,#2487,#325,.T.);
#1917=EDGE_CURVE('',#2486,#2480,#2852,.T.);
#1918=EDGE_CURVE('',#2487,#2483,#2853,.T.);
#1919=EDGE_CURVE('',#2488,#2488,#595,.T.);
#1920=EDGE_CURVE('',#2489,#2489,#326,.F.);
#1921=EDGE_CURVE('',#2490,#2490,#596,.T.);
#1922=EDGE_CURVE('',#2491,#2491,#327,.T.);
#1923=EDGE_CURVE('',#2492,#2492,#328,.T.);
#1924=EDGE_CURVE('',#2493,#2493,#597,.T.);
#1925=EDGE_CURVE('',#2494,#2494,#329,.T.);
#1926=EDGE_CURVE('',#2495,#2495,#598,.T.);
#1927=EDGE_CURVE('',#2496,#2496,#330,.T.);
#1928=EDGE_CURVE('',#2497,#2497,#331,.T.);
#1929=EDGE_CURVE('',#2498,#2498,#332,.T.);
#1930=EDGE_CURVE('',#2499,#2499,#333,.T.);
#1931=EDGE_CURVE('',#2500,#2500,#334,.T.);
#1932=EDGE_CURVE('',#2501,#2501,#335,.T.);
#1933=EDGE_CURVE('',#2502,#2502,#336,.T.);
#1934=EDGE_CURVE('',#2503,#2503,#337,.T.);
#1935=EDGE_CURVE('',#2504,#2504,#338,.T.);
#1936=EDGE_CURVE('',#2505,#2505,#339,.T.);
#1937=EDGE_CURVE('',#2506,#2506,#340,.T.);
#1938=EDGE_CURVE('',#2507,#2507,#341,.T.);
#1939=EDGE_CURVE('',#2508,#2508,#342,.T.);
#1940=EDGE_CURVE('',#2509,#2509,#343,.T.);
#1941=EDGE_CURVE('',#2510,#2510,#344,.T.);
#1942=EDGE_CURVE('',#2511,#2511,#345,.T.);
#1943=EDGE_CURVE('',#2512,#2512,#346,.T.);
#1944=EDGE_CURVE('',#2513,#2513,#347,.T.);
#1945=EDGE_CURVE('',#2514,#2514,#348,.T.);
#1946=EDGE_CURVE('',#2515,#2515,#349,.T.);
#1947=EDGE_CURVE('',#2516,#2516,#350,.T.);
#1948=EDGE_CURVE('',#2517,#2517,#351,.T.);
#1949=EDGE_CURVE('',#2518,#2518,#352,.T.);
#1950=EDGE_CURVE('',#2519,#2519,#353,.T.);
#1951=EDGE_CURVE('',#2520,#2521,#2854,.T.);
#1952=EDGE_CURVE('',#2521,#2522,#354,.T.);
#1953=EDGE_CURVE('',#2523,#2522,#2855,.T.);
#1954=EDGE_CURVE('',#2523,#2520,#355,.F.);
#1955=EDGE_CURVE('',#2523,#2524,#599,.T.);
#1956=EDGE_CURVE('',#2525,#2524,#356,.T.);
#1957=EDGE_CURVE('',#2520,#2525,#600,.T.);
#1958=EDGE_CURVE('',#2526,#2522,#601,.F.);
#1959=EDGE_CURVE('',#2527,#2521,#602,.F.);
#1960=EDGE_CURVE('',#2526,#2527,#357,.F.);
#1961=EDGE_CURVE('',#2528,#2529,#41,.T.);
#1962=EDGE_CURVE('',#2524,#2529,#2856,.F.);
#1963=EDGE_CURVE('',#2528,#2523,#2857,.T.);
#1964=EDGE_CURVE('',#2530,#2531,#42,.F.);
#1965=EDGE_CURVE('',#2522,#2531,#2858,.T.);
#1966=EDGE_CURVE('',#2530,#2526,#2859,.F.);
#1967=EDGE_CURVE('',#2532,#2525,#2860,.F.);
#1968=EDGE_CURVE('',#2533,#2532,#43,.T.);
#1969=EDGE_CURVE('',#2520,#2533,#2861,.T.);
#1970=EDGE_CURVE('',#2534,#2521,#2862,.T.);
#1971=EDGE_CURVE('',#2535,#2534,#44,.F.);
#1972=EDGE_CURVE('',#2527,#2535,#2863,.F.);
#1973=EDGE_CURVE('',#2536,#2537,#358,.F.);
#1974=EDGE_CURVE('',#2531,#2536,#2864,.F.);
#1975=EDGE_CURVE('',#2537,#2530,#2865,.T.);
#1976=EDGE_CURVE('',#2538,#2539,#359,.F.);
#1977=EDGE_CURVE('',#2529,#2538,#2866,.F.);
#1978=EDGE_CURVE('',#2539,#2528,#2867,.T.);
#1979=EDGE_CURVE('',#2539,#2536,#2868,.T.);
#1980=EDGE_CURVE('',#2531,#2528,#2869,.T.);
#1981=EDGE_CURVE('',#2540,#2541,#2870,.T.);
#1982=EDGE_CURVE('',#2542,#2540,#360,.T.);
#1983=EDGE_CURVE('',#2543,#2542,#2871,.T.);
#1984=EDGE_CURVE('',#2543,#2541,#361,.T.);
#1985=EDGE_CURVE('',#2544,#2545,#362,.F.);
#1986=EDGE_CURVE('',#2544,#2546,#603,.T.);
#1987=EDGE_CURVE('',#2547,#2546,#363,.T.);
#1988=EDGE_CURVE('',#2547,#2545,#604,.T.);
#1989=EDGE_CURVE('',#2547,#2540,#2872,.F.);
#1990=EDGE_CURVE('',#2542,#2546,#2873,.T.);
#1991=EDGE_CURVE('',#2548,#2549,#364,.F.);
#1992=EDGE_CURVE('',#2548,#2550,#605,.T.);
#1993=EDGE_CURVE('',#2551,#2550,#365,.T.);
#1994=EDGE_CURVE('',#2551,#2549,#606,.T.);
#1995=EDGE_CURVE('',#2552,#2553,#2874,.T.);
#1996=EDGE_CURVE('',#2552,#2554,#366,.T.);
#1997=EDGE_CURVE('',#2555,#2554,#2875,.T.);
#1998=EDGE_CURVE('',#2553,#2555,#367,.T.);
#1999=EDGE_CURVE('',#2552,#2548,#2876,.T.);
#2000=EDGE_CURVE('',#2549,#2554,#2877,.F.);
#2001=EDGE_CURVE('',#2555,#2541,#2878,.F.);
#2002=EDGE_CURVE('',#2543,#2553,#2879,.T.);
#2003=EDGE_CURVE('',#2556,#2557,#368,.F.);
#2004=EDGE_CURVE('',#2535,#2556,#2880,.F.);
#2005=EDGE_CURVE('',#2557,#2534,#2881,.T.);
#2006=EDGE_CURVE('',#2558,#2559,#369,.F.);
#2007=EDGE_CURVE('',#2533,#2558,#2882,.F.);
#2008=EDGE_CURVE('',#2559,#2532,#2883,.T.);
#2009=EDGE_CURVE('',#2558,#2557,#2884,.T.);
#2010=EDGE_CURVE('',#2534,#2533,#2885,.T.);
#2011=EDGE_CURVE('',#2556,#2551,#2886,.T.);
#2012=EDGE_CURVE('',#2550,#2537,#2887,.T.);
#2013=EDGE_CURVE('',#2559,#2545,#2888,.T.);
#2014=EDGE_CURVE('',#2544,#2538,#2889,.T.);
#2015=EDGE_CURVE('',#2560,#2560,#370,.T.);
#2016=EDGE_CURVE('',#2561,#2561,#371,.F.);
#2017=EDGE_CURVE('',#2562,#2562,#372,.T.);
#2018=EDGE_CURVE('',#2563,#2563,#373,.F.);
#2019=EDGE_CURVE('',#2564,#2565,#2890,.T.);
#2020=EDGE_CURVE('',#2565,#2566,#2891,.T.);
#2021=EDGE_CURVE('',#2566,#2567,#374,.F.);
#2022=EDGE_CURVE('',#2567,#2568,#2892,.T.);
#2023=EDGE_CURVE('',#2568,#2569,#2893,.F.);
#2024=EDGE_CURVE('',#2569,#2570,#375,.F.);
#2025=EDGE_CURVE('',#2570,#2571,#376,.T.);
#2026=EDGE_CURVE('',#2571,#2564,#377,.F.);
#2027=EDGE_CURVE('',#2572,#2573,#2894,.T.);
#2028=EDGE_CURVE('',#2572,#2574,#2895,.F.);
#2029=EDGE_CURVE('',#2574,#2575,#378,.T.);
#2030=EDGE_CURVE('',#2575,#2576,#379,.F.);
#2031=EDGE_CURVE('',#2576,#2577,#380,.T.);
#2032=EDGE_CURVE('',#2577,#2578,#2896,.T.);
#2033=EDGE_CURVE('',#2579,#2578,#2897,.T.);
#2034=EDGE_CURVE('',#2579,#2573,#381,.T.);
#2035=EDGE_CURVE('',#2580,#2581,#2898,.T.);
#2036=EDGE_CURVE('',#2580,#2582,#2899,.F.);
#2037=EDGE_CURVE('',#2582,#2583,#2900,.F.);
#2038=EDGE_CURVE('',#2583,#2581,#2901,.T.);
#2039=EDGE_CURVE('',#2584,#2585,#2902,.T.);
#2040=EDGE_CURVE('',#2585,#2586,#2903,.T.);
#2041=EDGE_CURVE('',#2586,#2587,#2904,.F.);
#2042=EDGE_CURVE('',#2587,#2584,#2905,.T.);
#2043=EDGE_CURVE('',#2588,#2589,#2906,.F.);
#2044=EDGE_CURVE('',#2588,#2590,#382,.T.);
#2045=EDGE_CURVE('',#2591,#2590,#2907,.T.);
#2046=EDGE_CURVE('',#2589,#2591,#383,.T.);
#2047=EDGE_CURVE('',#2592,#2592,#607,.T.);
#2048=EDGE_CURVE('',#2593,#2593,#384,.F.);
#2049=EDGE_CURVE('',#2594,#2594,#608,.T.);
#2050=EDGE_CURVE('',#2595,#2595,#385,.F.);
#2051=EDGE_CURVE('',#2596,#2597,#2908,.T.);
#2052=EDGE_CURVE('',#2598,#2596,#386,.T.);
#2053=EDGE_CURVE('',#2599,#2598,#2909,.F.);
#2054=EDGE_CURVE('',#2599,#2597,#387,.F.);
#2055=EDGE_CURVE('',#2596,#2590,#2910,.T.);
#2056=EDGE_CURVE('',#2588,#2598,#2911,.T.);
#2057=EDGE_CURVE('',#2600,#2601,#388,.T.);
#2058=EDGE_CURVE('',#2601,#2602,#2912,.F.);
#2059=EDGE_CURVE('',#2602,#2603,#389,.T.);
#2060=EDGE_CURVE('',#2603,#2600,#2913,.T.);
#2061=EDGE_CURVE('',#2602,#2589,#2914,.T.);
#2062=EDGE_CURVE('',#2591,#2603,#2915,.T.);
#2063=EDGE_CURVE('',#2568,#2585,#390,.F.);
#2064=EDGE_CURVE('',#2584,#2569,#391,.T.);
#2065=EDGE_CURVE('',#2586,#2578,#392,.F.);
#2066=EDGE_CURVE('',#2577,#2587,#393,.T.);
#2067=EDGE_CURVE('',#2580,#2565,#394,.F.);
#2068=EDGE_CURVE('',#2582,#2564,#395,.T.);
#2069=EDGE_CURVE('',#2572,#2581,#396,.F.);
#2070=EDGE_CURVE('',#2574,#2583,#397,.T.);
#2071=EDGE_CURVE('',#2597,#2579,#609,.T.);
#2072=EDGE_CURVE('',#2573,#2599,#610,.T.);
#2073=EDGE_CURVE('',#2567,#2600,#611,.T.);
#2074=EDGE_CURVE('',#2601,#2566,#612,.T.);
#2075=EDGE_CURVE('',#2604,#2605,#2916,.F.);
#2076=EDGE_CURVE('',#2605,#2606,#398,.T.);
#2077=EDGE_CURVE('',#2606,#2607,#399,.T.);
#2078=EDGE_CURVE('',#2607,#2608,#400,.T.);
#2079=EDGE_CURVE('',#2608,#2609,#2917,.F.);
#2080=EDGE_CURVE('',#2609,#2610,#401,.T.);
#2081=EDGE_CURVE('',#2610,#2611,#402,.T.);
#2082=EDGE_CURVE('',#2611,#2604,#403,.T.);
#2083=EDGE_CURVE('',#2612,#2613,#2918,.F.);
#2084=EDGE_CURVE('',#2613,#2614,#404,.F.);
#2085=EDGE_CURVE('',#2614,#2615,#405,.F.);
#2086=EDGE_CURVE('',#2615,#2616,#406,.F.);
#2087=EDGE_CURVE('',#2616,#2617,#2919,.F.);
#2088=EDGE_CURVE('',#2617,#2618,#407,.F.);
#2089=EDGE_CURVE('',#2618,#2619,#408,.F.);
#2090=EDGE_CURVE('',#2619,#2612,#409,.F.);
#2091=EDGE_CURVE('',#2620,#2621,#410,.F.);
#2092=EDGE_CURVE('',#2621,#2622,#411,.T.);
#2093=EDGE_CURVE('',#2622,#2623,#2920,.T.);
#2094=EDGE_CURVE('',#2623,#2624,#412,.T.);
#2095=EDGE_CURVE('',#2624,#2625,#413,.F.);
#2096=EDGE_CURVE('',#2625,#2620,#414,.T.);
#2097=EDGE_CURVE('',#2626,#2626,#415,.F.);
#2098=EDGE_CURVE('',#2627,#2628,#2921,.T.);
#2099=EDGE_CURVE('',#2627,#2629,#416,.T.);
#2100=EDGE_CURVE('',#2629,#2630,#613,.T.);
#2101=EDGE_CURVE('',#2630,#2631,#417,.T.);
#2102=EDGE_CURVE('',#2631,#2632,#2922,.T.);
#2103=EDGE_CURVE('',#2632,#2633,#418,.F.);
#2104=EDGE_CURVE('',#2633,#2634,#614,.T.);
#2105=EDGE_CURVE('',#2634,#2628,#419,.F.);
#2106=EDGE_CURVE('',#2635,#2636,#615,.T.);
#2107=EDGE_CURVE('',#2636,#2637,#420,.T.);
#2108=EDGE_CURVE('',#2637,#2638,#2923,.T.);
#2109=EDGE_CURVE('',#2638,#2639,#421,.F.);
#2110=EDGE_CURVE('',#2639,#2640,#616,.T.);
#2111=EDGE_CURVE('',#2640,#2641,#422,.F.);
#2112=EDGE_CURVE('',#2642,#2641,#2924,.T.);
#2113=EDGE_CURVE('',#2642,#2635,#423,.T.);
#2114=EDGE_CURVE('',#2643,#2644,#424,.T.);
#2115=EDGE_CURVE('',#2644,#2645,#425,.F.);
#2116=EDGE_CURVE('',#2645,#2646,#2925,.F.);
#2117=EDGE_CURVE('',#2646,#2647,#426,.F.);
#2118=EDGE_CURVE('',#2647,#2648,#427,.T.);
#2119=EDGE_CURVE('',#2648,#2643,#428,.F.);
#2120=EDGE_CURVE('',#2649,#2649,#429,.T.);
#2121=EDGE_CURVE('',#2650,#2651,#2926,.T.);
#2122=EDGE_CURVE('',#2651,#2652,#430,.T.);
#2123=EDGE_CURVE('',#2652,#2653,#431,.T.);
#2124=EDGE_CURVE('',#2653,#2654,#432,.T.);
#2125=EDGE_CURVE('',#2654,#2655,#2927,.T.);
#2126=EDGE_CURVE('',#2655,#2656,#433,.T.);
#2127=EDGE_CURVE('',#2656,#2657,#434,.T.);
#2128=EDGE_CURVE('',#2657,#2650,#435,.T.);
#2129=EDGE_CURVE('',#2658,#2659,#2928,.T.);
#2130=EDGE_CURVE('',#2659,#2660,#436,.F.);
#2131=EDGE_CURVE('',#2660,#2661,#437,.F.);
#2132=EDGE_CURVE('',#2661,#2662,#438,.F.);
#2133=EDGE_CURVE('',#2662,#2663,#2929,.T.);
#2134=EDGE_CURVE('',#2663,#2664,#439,.F.);
#2135=EDGE_CURVE('',#2664,#2665,#440,.F.);
#2136=EDGE_CURVE('',#2665,#2658,#441,.F.);
#2137=EDGE_CURVE('',#2666,#2667,#442,.T.);
#2138=EDGE_CURVE('',#2667,#2668,#2930,.T.);
#2139=EDGE_CURVE('',#2668,#2669,#443,.F.);
#2140=EDGE_CURVE('',#2669,#2670,#617,.T.);
#2141=EDGE_CURVE('',#2670,#2671,#444,.F.);
#2142=EDGE_CURVE('',#2672,#2671,#2931,.T.);
#2143=EDGE_CURVE('',#2672,#2673,#445,.T.);
#2144=EDGE_CURVE('',#2673,#2666,#618,.T.);
#2145=EDGE_CURVE('',#2637,#2627,#446,.F.);
#2146=EDGE_CURVE('',#2628,#2638,#447,.T.);
#2147=EDGE_CURVE('',#2674,#2675,#448,.F.);
#2148=EDGE_CURVE('',#2675,#2676,#2932,.F.);
#2149=EDGE_CURVE('',#2676,#2677,#449,.T.);
#2150=EDGE_CURVE('',#2677,#2678,#619,.T.);
#2151=EDGE_CURVE('',#2678,#2679,#450,.T.);
#2152=EDGE_CURVE('',#2679,#2680,#2933,.T.);
#2153=EDGE_CURVE('',#2680,#2681,#451,.F.);
#2154=EDGE_CURVE('',#2681,#2674,#620,.T.);
#2155=EDGE_CURVE('',#2679,#2642,#2934,.T.);
#2156=EDGE_CURVE('',#2641,#2680,#2935,.F.);
#2157=EDGE_CURVE('',#2631,#2672,#2936,.F.);
#2158=EDGE_CURVE('',#2671,#2632,#2937,.T.);
#2159=EDGE_CURVE('',#2682,#2682,#452,.T.);
#2160=EDGE_CURVE('',#2683,#2683,#453,.T.);
#2161=EDGE_CURVE('',#2684,#2685,#2938,.T.);
#2162=EDGE_CURVE('',#2685,#2686,#2939,.T.);
#2163=EDGE_CURVE('',#2687,#2686,#2940,.T.);
#2164=EDGE_CURVE('',#2687,#2684,#2941,.F.);
#2165=EDGE_CURVE('',#2688,#2689,#621,.T.);
#2166=EDGE_CURVE('',#2689,#2685,#454,.F.);
#2167=EDGE_CURVE('',#2684,#2690,#455,.F.);
#2168=EDGE_CURVE('',#2690,#2691,#2942,.T.);
#2169=EDGE_CURVE('',#2691,#2692,#456,.F.);
#2170=EDGE_CURVE('',#2692,#2693,#622,.T.);
#2171=EDGE_CURVE('',#2693,#2688,#623,.T.);
#2172=EDGE_CURVE('',#2694,#2695,#2943,.T.);
#2173=EDGE_CURVE('',#2695,#2691,#2944,.F.);
#2174=EDGE_CURVE('',#2690,#2694,#2945,.T.);
#2175=EDGE_CURVE('',#2686,#2696,#457,.F.);
#2176=EDGE_CURVE('',#2696,#2697,#624,.T.);
#2177=EDGE_CURVE('',#2697,#2695,#458,.F.);
#2178=EDGE_CURVE('',#2694,#2687,#459,.F.);
#2179=EDGE_CURVE('',#2698,#2699,#2946,.F.);
#2180=EDGE_CURVE('',#2699,#2700,#460,.T.);
#2181=EDGE_CURVE('',#2700,#2701,#2947,.T.);
#2182=EDGE_CURVE('',#2701,#2698,#461,.T.);
#2183=EDGE_CURVE('',#2702,#2703,#2948,.T.);
#2184=EDGE_CURVE('',#2703,#2704,#2949,.F.);
#2185=EDGE_CURVE('',#2705,#2704,#2950,.T.);
#2186=EDGE_CURVE('',#2705,#2702,#2951,.T.);
#2187=EDGE_CURVE('',#2706,#2707,#2952,.T.);
#2188=EDGE_CURVE('',#2707,#2708,#462,.T.);
#2189=EDGE_CURVE('',#2708,#2709,#625,.T.);
#2190=EDGE_CURVE('',#2709,#2703,#463,.T.);
#2191=EDGE_CURVE('',#2702,#2706,#464,.F.);
#2192=EDGE_CURVE('',#2710,#2711,#2953,.T.);
#2193=EDGE_CURVE('',#2711,#2707,#2954,.T.);
#2194=EDGE_CURVE('',#2706,#2710,#2955,.F.);
#2195=EDGE_CURVE('',#2712,#2713,#626,.T.);
#2196=EDGE_CURVE('',#2713,#2711,#465,.T.);
#2197=EDGE_CURVE('',#2710,#2705,#466,.F.);
#2198=EDGE_CURVE('',#2704,#2714,#467,.T.);
#2199=EDGE_CURVE('',#2714,#2715,#627,.T.);
#2200=EDGE_CURVE('',#2715,#2712,#628,.T.);
#2201=EDGE_CURVE('',#2716,#2717,#2956,.T.);
#2202=EDGE_CURVE('',#2717,#2718,#468,.T.);
#2203=EDGE_CURVE('',#2718,#2719,#2957,.F.);
#2204=EDGE_CURVE('',#2719,#2716,#469,.T.);
#2205=EDGE_CURVE('',#2720,#2721,#629,.T.);
#2206=EDGE_CURVE('',#2720,#2722,#470,.F.);
#2207=EDGE_CURVE('',#2722,#2615,#630,.T.);
#2208=EDGE_CURVE('',#2614,#2721,#631,.T.);
#2209=EDGE_CURVE('',#2723,#2724,#632,.T.);
#2210=EDGE_CURVE('',#2723,#2720,#2958,.T.);
#2211=EDGE_CURVE('',#2721,#2724,#633,.T.);
#2212=EDGE_CURVE('',#2664,#2725,#634,.T.);
#2213=EDGE_CURVE('',#2725,#2723,#471,.F.);
#2214=EDGE_CURVE('',#2724,#2665,#635,.T.);
#2215=EDGE_CURVE('',#2726,#2727,#636,.T.);
#2216=EDGE_CURVE('',#2726,#2728,#472,.F.);
#2217=EDGE_CURVE('',#2728,#2607,#637,.T.);
#2218=EDGE_CURVE('',#2606,#2727,#638,.T.);
#2219=EDGE_CURVE('',#2729,#2730,#639,.T.);
#2220=EDGE_CURVE('',#2729,#2726,#2959,.T.);
#2221=EDGE_CURVE('',#2727,#2730,#640,.T.);
#2222=EDGE_CURVE('',#2656,#2731,#641,.T.);
#2223=EDGE_CURVE('',#2731,#2729,#473,.F.);
#2224=EDGE_CURVE('',#2730,#2657,#642,.T.);
#2225=EDGE_CURVE('',#2618,#2732,#643,.T.);
#2226=EDGE_CURVE('',#2732,#2733,#474,.F.);
#2227=EDGE_CURVE('',#2733,#2661,#644,.T.);
#2228=EDGE_CURVE('',#2660,#2619,#645,.T.);
#2229=EDGE_CURVE('',#2610,#2734,#646,.T.);
#2230=EDGE_CURVE('',#2734,#2735,#475,.F.);
#2231=EDGE_CURVE('',#2735,#2653,#647,.T.);
#2232=EDGE_CURVE('',#2652,#2611,#648,.T.);
#2233=EDGE_CURVE('',#2687,#2701,#649,.T.);
#2234=EDGE_CURVE('',#2698,#2694,#650,.F.);
#2235=EDGE_CURVE('',#2699,#2690,#651,.F.);
#2236=EDGE_CURVE('',#2684,#2700,#652,.T.);
#2237=EDGE_CURVE('',#2736,#2736,#476,.F.);
#2238=EDGE_CURVE('',#2737,#2737,#477,.T.);
#2239=EDGE_CURVE('',#2738,#2738,#478,.F.);
#2240=EDGE_CURVE('',#2739,#2739,#479,.T.);
#2241=EDGE_CURVE('',#2660,#2709,#480,.T.);
#2242=EDGE_CURVE('',#2703,#2659,#653,.T.);
#2243=EDGE_CURVE('',#2704,#2658,#654,.T.);
#2244=EDGE_CURVE('',#2619,#2708,#481,.T.);
#2245=EDGE_CURVE('',#2714,#2665,#482,.T.);
#2246=EDGE_CURVE('',#2612,#2707,#655,.F.);
#2247=EDGE_CURVE('',#2715,#2724,#656,.T.);
#2248=EDGE_CURVE('',#2613,#2711,#657,.F.);
#2249=EDGE_CURVE('',#2712,#2721,#658,.F.);
#2250=EDGE_CURVE('',#2614,#2713,#483,.T.);
#2251=EDGE_CURVE('',#2666,#2570,#484,.T.);
#2252=EDGE_CURVE('',#2569,#2667,#485,.F.);
#2253=EDGE_CURVE('',#2733,#2666,#486,.F.);
#2254=EDGE_CURVE('',#2661,#2673,#487,.T.);
#2255=EDGE_CURVE('',#2662,#2672,#488,.T.);
#2256=EDGE_CURVE('',#2663,#2631,#489,.T.);
#2257=EDGE_CURVE('',#2664,#2630,#490,.T.);
#2258=EDGE_CURVE('',#2629,#2725,#491,.T.);
#2259=EDGE_CURVE('',#2676,#2564,#492,.T.);
#2260=EDGE_CURVE('',#2571,#2677,#493,.F.);
#2261=EDGE_CURVE('',#2677,#2732,#494,.T.);
#2262=EDGE_CURVE('',#2678,#2618,#495,.T.);
#2263=EDGE_CURVE('',#2679,#2617,#496,.T.);
#2264=EDGE_CURVE('',#2642,#2616,#497,.T.);
#2265=EDGE_CURVE('',#2635,#2615,#498,.T.);
#2266=EDGE_CURVE('',#2722,#2636,#499,.F.);
#2267=EDGE_CURVE('',#2652,#2697,#500,.T.);
#2268=EDGE_CURVE('',#2695,#2651,#659,.T.);
#2269=EDGE_CURVE('',#2691,#2650,#660,.T.);
#2270=EDGE_CURVE('',#2611,#2696,#501,.T.);
#2271=EDGE_CURVE('',#2692,#2657,#502,.T.);
#2272=EDGE_CURVE('',#2604,#2686,#661,.F.);
#2273=EDGE_CURVE('',#2693,#2730,#662,.T.);
#2274=EDGE_CURVE('',#2605,#2685,#663,.F.);
#2275=EDGE_CURVE('',#2688,#2727,#664,.F.);
#2276=EDGE_CURVE('',#2606,#2689,#503,.T.);
#2277=EDGE_CURVE('',#2674,#2575,#504,.F.);
#2278=EDGE_CURVE('',#2574,#2675,#505,.T.);
#2279=EDGE_CURVE('',#2735,#2674,#506,.F.);
#2280=EDGE_CURVE('',#2653,#2681,#507,.T.);
#2281=EDGE_CURVE('',#2654,#2680,#508,.T.);
#2282=EDGE_CURVE('',#2655,#2641,#509,.T.);
#2283=EDGE_CURVE('',#2656,#2640,#510,.T.);
#2284=EDGE_CURVE('',#2639,#2731,#511,.T.);
#2285=EDGE_CURVE('',#2576,#2669,#512,.T.);
#2286=EDGE_CURVE('',#2668,#2577,#513,.F.);
#2287=EDGE_CURVE('',#2669,#2734,#514,.T.);
#2288=EDGE_CURVE('',#2670,#2610,#515,.T.);
#2289=EDGE_CURVE('',#2671,#2609,#516,.T.);
#2290=EDGE_CURVE('',#2632,#2608,#517,.T.);
#2291=EDGE_CURVE('',#2633,#2607,#518,.T.);
#2292=EDGE_CURVE('',#2728,#2634,#519,.F.);
#2293=EDGE_CURVE('',#2716,#2710,#665,.F.);
#2294=EDGE_CURVE('',#2705,#2719,#666,.T.);
#2295=EDGE_CURVE('',#2702,#2718,#667,.T.);
#2296=EDGE_CURVE('',#2717,#2706,#668,.F.);
#2297=EDGE_CURVE('',#2734,#2576,#520,.T.);
#2298=EDGE_CURVE('',#2735,#2575,#521,.T.);
#2299=EDGE_CURVE('',#2667,#2584,#522,.T.);
#2300=EDGE_CURVE('',#2668,#2587,#523,.T.);
#2301=EDGE_CURVE('',#2582,#2676,#524,.T.);
#2302=EDGE_CURVE('',#2583,#2675,#525,.T.);
#2303=EDGE_CURVE('',#2732,#2571,#526,.T.);
#2304=EDGE_CURVE('',#2733,#2570,#527,.T.);
#2305=EDGE_CURVE('',#2627,#2625,#528,.T.);
#2306=EDGE_CURVE('',#2620,#2637,#529,.T.);
#2307=EDGE_CURVE('',#2621,#2636,#530,.T.);
#2308=EDGE_CURVE('',#2629,#2624,#531,.T.);
#2309=EDGE_CURVE('',#2621,#2722,#532,.T.);
#2310=EDGE_CURVE('',#2725,#2624,#533,.T.);
#2311=EDGE_CURVE('',#2622,#2720,#669,.F.);
#2312=EDGE_CURVE('',#2723,#2623,#670,.T.);
#2313=EDGE_CURVE('',#2643,#2628,#534,.T.);
#2314=EDGE_CURVE('',#2638,#2648,#535,.T.);
#2315=EDGE_CURVE('',#2639,#2647,#536,.T.);
#2316=EDGE_CURVE('',#2644,#2634,#537,.T.);
#2317=EDGE_CURVE('',#2731,#2647,#538,.T.);
#2318=EDGE_CURVE('',#2644,#2728,#539,.T.);
#2319=EDGE_CURVE('',#2729,#2646,#671,.T.);
#2320=EDGE_CURVE('',#2645,#2726,#672,.F.);
#2321=EDGE_CURVE('',#2740,#2741,#2960,.T.);
#2322=EDGE_CURVE('',#2742,#2740,#2961,.T.);
#2323=EDGE_CURVE('',#2742,#2743,#2962,.T.);
#2324=EDGE_CURVE('',#2741,#2743,#2963,.T.);
#2325=EDGE_CURVE('',#2744,#2740,#540,.T.);
#2326=EDGE_CURVE('',#2741,#2745,#541,.T.);
#2327=EDGE_CURVE('',#2745,#2744,#2964,.F.);
#2328=EDGE_CURVE('',#2746,#2742,#542,.T.);
#2329=EDGE_CURVE('',#2747,#2746,#2965,.F.);
#2330=EDGE_CURVE('',#2743,#2747,#543,.T.);
#2331=EDGE_CURVE('',#2747,#2745,#2966,.T.);
#2332=EDGE_CURVE('',#2744,#2746,#2967,.T.);
#2333=EDGE_CURVE('',#2748,#2748,#544,.T.);
#2334=EDGE_CURVE('',#2749,#2749,#545,.T.);
#2335=EDGE_CURVE('',#2750,#2750,#546,.T.);
#2336=EDGE_CURVE('',#2751,#2751,#547,.T.);
#2337=EDGE_CURVE('',#2752,#2752,#548,.T.);
#2338=EDGE_CURVE('',#2753,#2753,#549,.T.);
#2339=EDGE_CURVE('',#2754,#2754,#550,.T.);
#2340=EDGE_CURVE('',#2755,#2756,#2968,.T.);
#2341=EDGE_CURVE('',#2757,#2756,#551,.T.);
#2342=EDGE_CURVE('',#2757,#2758,#2969,.T.);
#2343=EDGE_CURVE('',#2755,#2758,#552,.T.);
#2344=EDGE_CURVE('',#2759,#2759,#553,.T.);
#2345=EDGE_CURVE('',#2760,#2760,#554,.T.);
#2346=EDGE_CURVE('',#2761,#2762,#2970,.T.);
#2347=EDGE_CURVE('',#2763,#2761,#555,.T.);
#2348=EDGE_CURVE('',#2764,#2763,#2971,.T.);
#2349=EDGE_CURVE('',#2760,#2764,#2972,.T.);
#2350=EDGE_CURVE('',#2762,#2760,#2973,.T.);
#2351=EDGE_CURVE('',#2765,#2766,#2974,.T.);
#2352=EDGE_CURVE('',#2765,#2756,#673,.T.);
#2353=EDGE_CURVE('',#2755,#2767,#674,.T.);
#2354=EDGE_CURVE('',#2761,#2767,#2975,.T.);
#2355=EDGE_CURVE('',#2762,#2768,#2976,.T.);
#2356=EDGE_CURVE('',#2768,#2769,#45,.T.);
#2357=EDGE_CURVE('',#2769,#2766,#2977,.T.);
#2358=EDGE_CURVE('',#2763,#2770,#2978,.T.);
#2359=EDGE_CURVE('',#2770,#2767,#675,.T.);
#2360=EDGE_CURVE('',#2757,#2771,#676,.T.);
#2361=EDGE_CURVE('',#2771,#2772,#2979,.T.);
#2362=EDGE_CURVE('',#2772,#2773,#2980,.T.);
#2363=EDGE_CURVE('',#2774,#2773,#46,.T.);
#2364=EDGE_CURVE('',#2764,#2774,#2981,.T.);
#2365=EDGE_CURVE('',#2770,#2758,#677,.T.);
#2366=EDGE_CURVE('',#2768,#2774,#2982,.T.);
#2367=EDGE_CURVE('',#2775,#2776,#678,.T.);
#2368=EDGE_CURVE('',#2776,#2775,#679,.T.);
#2369=EDGE_CURVE('',#2777,#2777,#556,.T.);
#2370=EDGE_CURVE('',#2778,#2778,#557,.T.);
#2371=EDGE_CURVE('',#2769,#2773,#2983,.T.);
#2372=EDGE_CURVE('',#2772,#2779,#558,.T.);
#2373=EDGE_CURVE('',#2780,#2779,#559,.T.);
#2374=EDGE_CURVE('',#2780,#2766,#560,.T.);
#2375=EDGE_CURVE('',#2765,#2781,#680,.T.);
#2376=EDGE_CURVE('',#2781,#2780,#2984,.T.);
#2377=EDGE_CURVE('',#2781,#2782,#681,.T.);
#2378=EDGE_CURVE('',#2782,#2771,#682,.T.);
#2379=EDGE_CURVE('',#2782,#2779,#2985,.T.);
#2380=EDGE_CURVE('',#2776,#2775,#47,.T.);
#2381=EDGE_CURVE('',#2783,#2784,#48,.T.);
#2382=EDGE_CURVE('',#2783,#2784,#683,.T.);
#2383=EDGE_CURVE('',#2785,#2786,#49,.T.);
#2384=EDGE_CURVE('',#2786,#2785,#684,.T.);
#2385=EDGE_CURVE('',#2787,#2787,#561,.T.);
#2386=EDGE_CURVE('',#2788,#2788,#562,.F.);
#2387=EDGE_CURVE('',#2789,#2789,#563,.T.);
#2388=EDGE_CURVE('',#2790,#2783,#564,.T.);
#2389=EDGE_CURVE('',#2784,#2791,#565,.T.);
#2390=EDGE_CURVE('',#2791,#2790,#685,.T.);
#2391=EDGE_CURVE('',#2792,#2793,#566,.T.);
#2392=EDGE_CURVE('',#2793,#2794,#686,.T.);
#2393=EDGE_CURVE('',#2794,#2795,#567,.T.);
#2394=EDGE_CURVE('',#2795,#2792,#687,.T.);
#2395=EDGE_CURVE('',#2794,#2793,#50,.F.);
#2396=EDGE_CURVE('',#2792,#2795,#51,.T.);
#2397=EDGE_CURVE('',#2791,#2790,#52,.F.);
#2398=EDGE_CURVE('',#2796,#2796,#568,.F.);
#2399=EDGE_CURVE('',#2797,#2797,#569,.T.);
#2400=EDGE_CURVE('',#2798,#2786,#688,.T.);
#2401=EDGE_CURVE('',#2785,#2799,#570,.T.);
#2402=EDGE_CURVE('',#2799,#2798,#689,.T.);
#2403=EDGE_CURVE('',#2800,#2800,#690,.T.);
#2404=EDGE_CURVE('',#2798,#2799,#53,.T.);
#2405=EDGE_CURVE('',#2801,#2802,#2986,.T.);
#2406=EDGE_CURVE('',#2803,#2802,#571,.T.);
#2407=EDGE_CURVE('',#2803,#2804,#2987,.T.);
#2408=EDGE_CURVE('',#2752,#2804,#2988,.T.);
#2409=EDGE_CURVE('',#2801,#2752,#2989,.T.);
#2410=EDGE_CURVE('',#2805,#2805,#572,.T.);
#2411=EDGE_CURVE('',#2806,#2806,#54,.F.);
#2412=EDGE_CURVE('',#2807,#2808,#55,.T.);
#2413=EDGE_CURVE('',#2809,#2807,#2990,.T.);
#2414=EDGE_CURVE('',#2810,#2809,#2991,.T.);
#2415=EDGE_CURVE('',#2811,#2810,#691,.T.);
#2416=EDGE_CURVE('',#2812,#2811,#2992,.T.);
#2417=EDGE_CURVE('',#2813,#2812,#692,.T.);
#2418=EDGE_CURVE('',#2802,#2813,#2993,.T.);
#2419=EDGE_CURVE('',#2808,#2801,#2994,.T.);
#2420=EDGE_CURVE('',#2803,#2814,#2995,.T.);
#2421=EDGE_CURVE('',#2813,#2814,#693,.T.);
#2422=EDGE_CURVE('',#2815,#2814,#694,.T.);
#2423=EDGE_CURVE('',#2816,#2815,#2996,.T.);
#2424=EDGE_CURVE('',#2817,#2816,#695,.T.);
#2425=EDGE_CURVE('',#2817,#2818,#2997,.T.);
#2426=EDGE_CURVE('',#2819,#2818,#2998,.T.);
#2427=EDGE_CURVE('',#2819,#2820,#56,.T.);
#2428=EDGE_CURVE('',#2820,#2804,#2999,.T.);
#2429=EDGE_CURVE('',#2820,#2808,#3000,.T.);
#2430=EDGE_CURVE('',#2821,#2821,#573,.T.);
#2431=EDGE_CURVE('',#2819,#2807,#3001,.T.);
#2432=EDGE_CURVE('',#2818,#2822,#574,.T.);
#2433=EDGE_CURVE('',#2823,#2822,#575,.T.);
#2434=EDGE_CURVE('',#2823,#2809,#576,.T.);
#2435=EDGE_CURVE('',#2824,#2823,#3002,.T.);
#2436=EDGE_CURVE('',#2810,#2824,#696,.T.);
#2437=EDGE_CURVE('',#2811,#2816,#577,.T.);
#2438=EDGE_CURVE('',#2825,#2824,#697,.T.);
#2439=EDGE_CURVE('',#2825,#2817,#698,.T.);
#2440=EDGE_CURVE('',#2815,#2812,#578,.T.);
#2441=EDGE_CURVE('',#2825,#2822,#3003,.T.);
#2442=EDGE_CURVE('',#2826,#2827,#3004,.T.);
#2443=EDGE_CURVE('',#2826,#2828,#579,.T.);
#2444=EDGE_CURVE('',#2829,#2828,#3005,.T.);
#2445=EDGE_CURVE('',#2827,#2829,#580,.T.);
#2446=EDGE_CURVE('',#2830,#2829,#3006,.T.);
#2447=EDGE_CURVE('',#2830,#2831,#581,.T.);
#2448=EDGE_CURVE('',#2827,#2831,#3007,.F.);
#2449=EDGE_CURVE('',#2832,#2833,#582,.T.);
#2450=EDGE_CURVE('',#2832,#2828,#3008,.T.);
#2451=EDGE_CURVE('',#2826,#2833,#3009,.F.);
#2452=EDGE_CURVE('',#2832,#2830,#3010,.T.);
#2453=EDGE_CURVE('',#2831,#2833,#3011,.T.);
#2454=VERTEX_POINT('',#6405);
#2455=VERTEX_POINT('',#6406);
#2456=VERTEX_POINT('',#6411);
#2457=VERTEX_POINT('',#6416);
#2458=VERTEX_POINT('',#6418);
#2459=VERTEX_POINT('',#6422);
#2460=VERTEX_POINT('',#6423);
#2461=VERTEX_POINT('',#6428);
#2462=VERTEX_POINT('',#6436);
#2463=VERTEX_POINT('',#6437);
#2464=VERTEX_POINT('',#6442);
#2465=VERTEX_POINT('',#6450);
#2466=VERTEX_POINT('',#6451);
#2467=VERTEX_POINT('',#6456);
#2468=VERTEX_POINT('',#6464);
#2469=VERTEX_POINT('',#6465);
#2470=VERTEX_POINT('',#6470);
#2471=VERTEX_POINT('',#6481);
#2472=VERTEX_POINT('',#6489);
#2473=VERTEX_POINT('',#6492);
#2474=VERTEX_POINT('',#6494);
#2475=VERTEX_POINT('',#6497);
#2476=VERTEX_POINT('',#6516);
#2477=VERTEX_POINT('',#6518);
#2478=VERTEX_POINT('',#6521);
#2479=VERTEX_POINT('',#6523);
#2480=VERTEX_POINT('',#6529);
#2481=VERTEX_POINT('',#6530);
#2482=VERTEX_POINT('',#6532);
#2483=VERTEX_POINT('',#6534);
#2484=VERTEX_POINT('',#6538);
#2485=VERTEX_POINT('',#6540);
#2486=VERTEX_POINT('',#6544);
#2487=VERTEX_POINT('',#6546);
#2488=VERTEX_POINT('',#6574);
#2489=VERTEX_POINT('',#6576);
#2490=VERTEX_POINT('',#6599);
#2491=VERTEX_POINT('',#6601);
#2492=VERTEX_POINT('',#6603);
#2493=VERTEX_POINT('',#6625);
#2494=VERTEX_POINT('',#6628);
#2495=VERTEX_POINT('',#6648);
#2496=VERTEX_POINT('',#6650);
#2497=VERTEX_POINT('',#6653);
#2498=VERTEX_POINT('',#6656);
#2499=VERTEX_POINT('',#6659);
#2500=VERTEX_POINT('',#6662);
#2501=VERTEX_POINT('',#6665);
#2502=VERTEX_POINT('',#6668);
#2503=VERTEX_POINT('',#6671);
#2504=VERTEX_POINT('',#6674);
#2505=VERTEX_POINT('',#6677);
#2506=VERTEX_POINT('',#6680);
#2507=VERTEX_POINT('',#6683);
#2508=VERTEX_POINT('',#6686);
#2509=VERTEX_POINT('',#6689);
#2510=VERTEX_POINT('',#6692);
#2511=VERTEX_POINT('',#6695);
#2512=VERTEX_POINT('',#6698);
#2513=VERTEX_POINT('',#6704);
#2514=VERTEX_POINT('',#6708);
#2515=VERTEX_POINT('',#6711);
#2516=VERTEX_POINT('',#6718);
#2517=VERTEX_POINT('',#6720);
#2518=VERTEX_POINT('',#6723);
#2519=VERTEX_POINT('',#6725);
#2520=VERTEX_POINT('',#6731);
#2521=VERTEX_POINT('',#6732);
#2522=VERTEX_POINT('',#6734);
#2523=VERTEX_POINT('',#6736);
#2524=VERTEX_POINT('',#6744);
#2525=VERTEX_POINT('',#6746);
#2526=VERTEX_POINT('',#6758);
#2527=VERTEX_POINT('',#6764);
#2528=VERTEX_POINT('',#6768);
#2529=VERTEX_POINT('',#6769);
#2530=VERTEX_POINT('',#6774);
#2531=VERTEX_POINT('',#6775);
#2532=VERTEX_POINT('',#6780);
#2533=VERTEX_POINT('',#6782);
#2534=VERTEX_POINT('',#6786);
#2535=VERTEX_POINT('',#6788);
#2536=VERTEX_POINT('',#6792);
#2537=VERTEX_POINT('',#6793);
#2538=VERTEX_POINT('',#6798);
#2539=VERTEX_POINT('',#6799);
#2540=VERTEX_POINT('',#6807);
#2541=VERTEX_POINT('',#6808);
#2542=VERTEX_POINT('',#6810);
#2543=VERTEX_POINT('',#6812);
#2544=VERTEX_POINT('',#6816);
#2545=VERTEX_POINT('',#6817);
#2546=VERTEX_POINT('',#6823);
#2547=VERTEX_POINT('',#6825);
#2548=VERTEX_POINT('',#6836);
#2549=VERTEX_POINT('',#6837);
#2550=VERTEX_POINT('',#6843);
#2551=VERTEX_POINT('',#6845);
#2552=VERTEX_POINT('',#6853);
#2553=VERTEX_POINT('',#6854);
#2554=VERTEX_POINT('',#6856);
#2555=VERTEX_POINT('',#6858);
#2556=VERTEX_POINT('',#6868);
#2557=VERTEX_POINT('',#6869);
#2558=VERTEX_POINT('',#6874);
#2559=VERTEX_POINT('',#6875);
#2560=VERTEX_POINT('',#6889);
#2561=VERTEX_POINT('',#6892);
#2562=VERTEX_POINT('',#6895);
#2563=VERTEX_POINT('',#6898);
#2564=VERTEX_POINT('',#6905);
#2565=VERTEX_POINT('',#6906);
#2566=VERTEX_POINT('',#6908);
#2567=VERTEX_POINT('',#6910);
#2568=VERTEX_POINT('',#6912);
#2569=VERTEX_POINT('',#6914);
#2570=VERTEX_POINT('',#6916);
#2571=VERTEX_POINT('',#6918);
#2572=VERTEX_POINT('',#6922);
#2573=VERTEX_POINT('',#6923);
#2574=VERTEX_POINT('',#6925);
#2575=VERTEX_POINT('',#6927);
#2576=VERTEX_POINT('',#6929);
#2577=VERTEX_POINT('',#6931);
#2578=VERTEX_POINT('',#6933);
#2579=VERTEX_POINT('',#6935);
#2580=VERTEX_POINT('',#6939);
#2581=VERTEX_POINT('',#6940);
#2582=VERTEX_POINT('',#6942);
#2583=VERTEX_POINT('',#6944);
#2584=VERTEX_POINT('',#6948);
#2585=VERTEX_POINT('',#6949);
#2586=VERTEX_POINT('',#6951);
#2587=VERTEX_POINT('',#6953);
#2588=VERTEX_POINT('',#6957);
#2589=VERTEX_POINT('',#6958);
#2590=VERTEX_POINT('',#6960);
#2591=VERTEX_POINT('',#6962);
#2592=VERTEX_POINT('',#6984);
#2593=VERTEX_POINT('',#6986);
#2594=VERTEX_POINT('',#7007);
#2595=VERTEX_POINT('',#7009);
#2596=VERTEX_POINT('',#7012);
#2597=VERTEX_POINT('',#7013);
#2598=VERTEX_POINT('',#7015);
#2599=VERTEX_POINT('',#7017);
#2600=VERTEX_POINT('',#7024);
#2601=VERTEX_POINT('',#7025);
#2602=VERTEX_POINT('',#7027);
#2603=VERTEX_POINT('',#7029);
#2604=VERTEX_POINT('',#7070);
#2605=VERTEX_POINT('',#7071);
#2606=VERTEX_POINT('',#7073);
#2607=VERTEX_POINT('',#7075);
#2608=VERTEX_POINT('',#7077);
#2609=VERTEX_POINT('',#7079);
#2610=VERTEX_POINT('',#7081);
#2611=VERTEX_POINT('',#7083);
#2612=VERTEX_POINT('',#7087);
#2613=VERTEX_POINT('',#7088);
#2614=VERTEX_POINT('',#7090);
#2615=VERTEX_POINT('',#7092);
#2616=VERTEX_POINT('',#7094);
#2617=VERTEX_POINT('',#7096);
#2618=VERTEX_POINT('',#7098);
#2619=VERTEX_POINT('',#7100);
#2620=VERTEX_POINT('',#7104);
#2621=VERTEX_POINT('',#7105);
#2622=VERTEX_POINT('',#7107);
#2623=VERTEX_POINT('',#7109);
#2624=VERTEX_POINT('',#7111);
#2625=VERTEX_POINT('',#7113);
#2626=VERTEX_POINT('',#7116);
#2627=VERTEX_POINT('',#7119);
#2628=VERTEX_POINT('',#7120);
#2629=VERTEX_POINT('',#7122);
#2630=VERTEX_POINT('',#7130);
#2631=VERTEX_POINT('',#7132);
#2632=VERTEX_POINT('',#7134);
#2633=VERTEX_POINT('',#7136);
#2634=VERTEX_POINT('',#7144);
#2635=VERTEX_POINT('',#7154);
#2636=VERTEX_POINT('',#7155);
#2637=VERTEX_POINT('',#7157);
#2638=VERTEX_POINT('',#7159);
#2639=VERTEX_POINT('',#7161);
#2640=VERTEX_POINT('',#7169);
#2641=VERTEX_POINT('',#7171);
#2642=VERTEX_POINT('',#7173);
#2643=VERTEX_POINT('',#7177);
#2644=VERTEX_POINT('',#7178);
#2645=VERTEX_POINT('',#7180);
#2646=VERTEX_POINT('',#7182);
#2647=VERTEX_POINT('',#7184);
#2648=VERTEX_POINT('',#7186);
#2649=VERTEX_POINT('',#7189);
#2650=VERTEX_POINT('',#7192);
#2651=VERTEX_POINT('',#7193);
#2652=VERTEX_POINT('',#7195);
#2653=VERTEX_POINT('',#7197);
#2654=VERTEX_POINT('',#7199);
#2655=VERTEX_POINT('',#7201);
#2656=VERTEX_POINT('',#7203);
#2657=VERTEX_POINT('',#7205);
#2658=VERTEX_POINT('',#7209);
#2659=VERTEX_POINT('',#7210);
#2660=VERTEX_POINT('',#7212);
#2661=VERTEX_POINT('',#7214);
#2662=VERTEX_POINT('',#7216);
#2663=VERTEX_POINT('',#7218);
#2664=VERTEX_POINT('',#7220);
#2665=VERTEX_POINT('',#7222);
#2666=VERTEX_POINT('',#7226);
#2667=VERTEX_POINT('',#7227);
#2668=VERTEX_POINT('',#7229);
#2669=VERTEX_POINT('',#7231);
#2670=VERTEX_POINT('',#7237);
#2671=VERTEX_POINT('',#7239);
#2672=VERTEX_POINT('',#7241);
#2673=VERTEX_POINT('',#7243);
#2674=VERTEX_POINT('',#7254);
#2675=VERTEX_POINT('',#7255);
#2676=VERTEX_POINT('',#7257);
#2677=VERTEX_POINT('',#7259);
#2678=VERTEX_POINT('',#7265);
#2679=VERTEX_POINT('',#7267);
#2680=VERTEX_POINT('',#7269);
#2681=VERTEX_POINT('',#7271);
#2682=VERTEX_POINT('',#7285);
#2683=VERTEX_POINT('',#7287);
#2684=VERTEX_POINT('',#7290);
#2685=VERTEX_POINT('',#7291);
#2686=VERTEX_POINT('',#7293);
#2687=VERTEX_POINT('',#7295);
#2688=VERTEX_POINT('',#7302);
#2689=VERTEX_POINT('',#7303);
#2690=VERTEX_POINT('',#7306);
#2691=VERTEX_POINT('',#7308);
#2692=VERTEX_POINT('',#7310);
#2693=VERTEX_POINT('',#7315);
#2694=VERTEX_POINT('',#7322);
#2695=VERTEX_POINT('',#7323);
#2696=VERTEX_POINT('',#7328);
#2697=VERTEX_POINT('',#7333);
#2698=VERTEX_POINT('',#7338);
#2699=VERTEX_POINT('',#7339);
#2700=VERTEX_POINT('',#7341);
#2701=VERTEX_POINT('',#7343);
#2702=VERTEX_POINT('',#7347);
#2703=VERTEX_POINT('',#7348);
#2704=VERTEX_POINT('',#7350);
#2705=VERTEX_POINT('',#7352);
#2706=VERTEX_POINT('',#7356);
#2707=VERTEX_POINT('',#7357);
#2708=VERTEX_POINT('',#7359);
#2709=VERTEX_POINT('',#7364);
#2710=VERTEX_POINT('',#7369);
#2711=VERTEX_POINT('',#7370);
#2712=VERTEX_POINT('',#7378);
#2713=VERTEX_POINT('',#7379);
#2714=VERTEX_POINT('',#7383);
#2715=VERTEX_POINT('',#7388);
#2716=VERTEX_POINT('',#7395);
#2717=VERTEX_POINT('',#7396);
#2718=VERTEX_POINT('',#7398);
#2719=VERTEX_POINT('',#7400);
#2720=VERTEX_POINT('',#7407);
#2721=VERTEX_POINT('',#7408);
#2722=VERTEX_POINT('',#7410);
#2723=VERTEX_POINT('',#7427);
#2724=VERTEX_POINT('',#7428);
#2725=VERTEX_POINT('',#7441);
#2726=VERTEX_POINT('',#7453);
#2727=VERTEX_POINT('',#7454);
#2728=VERTEX_POINT('',#7456);
#2729=VERTEX_POINT('',#7473);
#2730=VERTEX_POINT('',#7474);
#2731=VERTEX_POINT('',#7487);
#2732=VERTEX_POINT('',#7500);
#2733=VERTEX_POINT('',#7502);
#2734=VERTEX_POINT('',#7518);
#2735=VERTEX_POINT('',#7520);
#2736=VERTEX_POINT('',#7556);
#2737=VERTEX_POINT('',#7558);
#2738=VERTEX_POINT('',#7561);
#2739=VERTEX_POINT('',#7563);
#2740=VERTEX_POINT('',#8031);
#2741=VERTEX_POINT('',#8032);
#2742=VERTEX_POINT('',#8034);
#2743=VERTEX_POINT('',#8036);
#2744=VERTEX_POINT('',#8040);
#2745=VERTEX_POINT('',#8042);
#2746=VERTEX_POINT('',#8046);
#2747=VERTEX_POINT('',#8048);
#2748=VERTEX_POINT('',#8058);
#2749=VERTEX_POINT('',#8060);
#2750=VERTEX_POINT('',#8063);
#2751=VERTEX_POINT('',#8065);
#2752=VERTEX_POINT('',#8071);
#2753=VERTEX_POINT('',#8073);
#2754=VERTEX_POINT('',#8076);
#2755=VERTEX_POINT('',#8078);
#2756=VERTEX_POINT('',#8079);
#2757=VERTEX_POINT('',#8081);
#2758=VERTEX_POINT('',#8083);
#2759=VERTEX_POINT('',#8087);
#2760=VERTEX_POINT('',#8089);
#2761=VERTEX_POINT('',#8092);
#2762=VERTEX_POINT('',#8093);
#2763=VERTEX_POINT('',#8095);
#2764=VERTEX_POINT('',#8097);
#2765=VERTEX_POINT('',#8102);
#2766=VERTEX_POINT('',#8103);
#2767=VERTEX_POINT('',#8116);
#2768=VERTEX_POINT('',#8119);
#2769=VERTEX_POINT('',#8121);
#2770=VERTEX_POINT('',#8125);
#2771=VERTEX_POINT('',#8155);
#2772=VERTEX_POINT('',#8157);
#2773=VERTEX_POINT('',#8159);
#2774=VERTEX_POINT('',#8161);
#2775=VERTEX_POINT('',#8180);
#2776=VERTEX_POINT('',#8181);
#2777=VERTEX_POINT('',#8192);
#2778=VERTEX_POINT('',#8194);
#2779=VERTEX_POINT('',#8199);
#2780=VERTEX_POINT('',#8201);
#2781=VERTEX_POINT('',#8208);
#2782=VERTEX_POINT('',#8233);
#2783=VERTEX_POINT('',#8244);
#2784=VERTEX_POINT('',#8245);
#2785=VERTEX_POINT('',#8257);
#2786=VERTEX_POINT('',#8258);
#2787=VERTEX_POINT('',#8271);
#2788=VERTEX_POINT('',#8274);
#2789=VERTEX_POINT('',#8276);
#2790=VERTEX_POINT('',#8278);
#2791=VERTEX_POINT('',#8280);
#2792=VERTEX_POINT('',#8291);
#2793=VERTEX_POINT('',#8292);
#2794=VERTEX_POINT('',#8302);
#2795=VERTEX_POINT('',#8304);
#2796=VERTEX_POINT('',#8320);
#2797=VERTEX_POINT('',#8322);
#2798=VERTEX_POINT('',#8327);
#2799=VERTEX_POINT('',#8329);
#2800=VERTEX_POINT('',#8350);
#2801=VERTEX_POINT('',#8356);
#2802=VERTEX_POINT('',#8357);
#2803=VERTEX_POINT('',#8359);
#2804=VERTEX_POINT('',#8361);
#2805=VERTEX_POINT('',#8366);
#2806=VERTEX_POINT('',#8371);
#2807=VERTEX_POINT('',#8375);
#2808=VERTEX_POINT('',#8376);
#2809=VERTEX_POINT('',#8378);
#2810=VERTEX_POINT('',#8380);
#2811=VERTEX_POINT('',#8387);
#2812=VERTEX_POINT('',#8389);
#2813=VERTEX_POINT('',#8395);
#2814=VERTEX_POINT('',#8400);
#2815=VERTEX_POINT('',#8430);
#2816=VERTEX_POINT('',#8432);
#2817=VERTEX_POINT('',#8438);
#2818=VERTEX_POINT('',#8440);
#2819=VERTEX_POINT('',#8442);
#2820=VERTEX_POINT('',#8444);
#2821=VERTEX_POINT('',#8450);
#2822=VERTEX_POINT('',#8455);
#2823=VERTEX_POINT('',#8457);
#2824=VERTEX_POINT('',#8461);
#2825=VERTEX_POINT('',#8490);
#2826=VERTEX_POINT('',#8508);
#2827=VERTEX_POINT('',#8509);
#2828=VERTEX_POINT('',#8511);
#2829=VERTEX_POINT('',#8513);
#2830=VERTEX_POINT('',#8517);
#2831=VERTEX_POINT('',#8519);
#2832=VERTEX_POINT('',#8523);
#2833=VERTEX_POINT('',#8524);
#2834=LINE('',#6404,#3012);
#2835=LINE('',#6417,#3013);
#2836=LINE('',#6419,#3014);
#2837=LINE('',#6421,#3015);
#2838=LINE('',#6433,#3016);
#2839=LINE('',#6435,#3017);
#2840=LINE('',#6447,#3018);
#2841=LINE('',#6449,#3019);
#2842=LINE('',#6461,#3020);
#2843=LINE('',#6463,#3021);
#2844=LINE('',#6475,#3022);
#2845=LINE('',#6486,#3023);
#2846=LINE('',#6531,#3024);
#2847=LINE('',#6535,#3025);
#2848=LINE('',#6537,#3026);
#2849=LINE('',#6539,#3027);
#2850=LINE('',#6541,#3028);
#2851=LINE('',#6545,#3029);
#2852=LINE('',#6549,#3030);
#2853=LINE('',#6550,#3031);
#2854=LINE('',#6730,#3032);
#2855=LINE('',#6735,#3033);
#2856=LINE('',#6770,#3034);
#2857=LINE('',#6771,#3035);
#2858=LINE('',#6776,#3036);
#2859=LINE('',#6777,#3037);
#2860=LINE('',#6779,#3038);
#2861=LINE('',#6783,#3039);
#2862=LINE('',#6785,#3040);
#2863=LINE('',#6789,#3041);
#2864=LINE('',#6794,#3042);
#2865=LINE('',#6795,#3043);
#2866=LINE('',#6800,#3044);
#2867=LINE('',#6801,#3045);
#2868=LINE('',#6803,#3046);
#2869=LINE('',#6804,#3047);
#2870=LINE('',#6806,#3048);
#2871=LINE('',#6811,#3049);
#2872=LINE('',#6832,#3050);
#2873=LINE('',#6833,#3051);
#2874=LINE('',#6852,#3052);
#2875=LINE('',#6857,#3053);
#2876=LINE('',#6861,#3054);
#2877=LINE('',#6862,#3055);
#2878=LINE('',#6864,#3056);
#2879=LINE('',#6865,#3057);
#2880=LINE('',#6870,#3058);
#2881=LINE('',#6871,#3059);
#2882=LINE('',#6876,#3060);
#2883=LINE('',#6877,#3061);
#2884=LINE('',#6879,#3062);
#2885=LINE('',#6880,#3063);
#2886=LINE('',#6882,#3064);
#2887=LINE('',#6883,#3065);
#2888=LINE('',#6885,#3066);
#2889=LINE('',#6886,#3067);
#2890=LINE('',#6904,#3068);
#2891=LINE('',#6907,#3069);
#2892=LINE('',#6911,#3070);
#2893=LINE('',#6913,#3071);
#2894=LINE('',#6921,#3072);
#2895=LINE('',#6924,#3073);
#2896=LINE('',#6932,#3074);
#2897=LINE('',#6934,#3075);
#2898=LINE('',#6938,#3076);
#2899=LINE('',#6941,#3077);
#2900=LINE('',#6943,#3078);
#2901=LINE('',#6945,#3079);
#2902=LINE('',#6947,#3080);
#2903=LINE('',#6950,#3081);
#2904=LINE('',#6952,#3082);
#2905=LINE('',#6954,#3083);
#2906=LINE('',#6956,#3084);
#2907=LINE('',#6961,#3085);
#2908=LINE('',#7011,#3086);
#2909=LINE('',#7016,#3087);
#2910=LINE('',#7020,#3088);
#2911=LINE('',#7021,#3089);
#2912=LINE('',#7026,#3090);
#2913=LINE('',#7030,#3091);
#2914=LINE('',#7032,#3092);
#2915=LINE('',#7033,#3093);
#2916=LINE('',#7069,#3094);
#2917=LINE('',#7078,#3095);
#2918=LINE('',#7086,#3096);
#2919=LINE('',#7095,#3097);
#2920=LINE('',#7108,#3098);
#2921=LINE('',#7118,#3099);
#2922=LINE('',#7133,#3100);
#2923=LINE('',#7158,#3101);
#2924=LINE('',#7172,#3102);
#2925=LINE('',#7181,#3103);
#2926=LINE('',#7191,#3104);
#2927=LINE('',#7200,#3105);
#2928=LINE('',#7208,#3106);
#2929=LINE('',#7217,#3107);
#2930=LINE('',#7228,#3108);
#2931=LINE('',#7240,#3109);
#2932=LINE('',#7256,#3110);
#2933=LINE('',#7268,#3111);
#2934=LINE('',#7278,#3112);
#2935=LINE('',#7279,#3113);
#2936=LINE('',#7281,#3114);
#2937=LINE('',#7282,#3115);
#2938=LINE('',#7289,#3116);
#2939=LINE('',#7292,#3117);
#2940=LINE('',#7294,#3118);
#2941=LINE('',#7296,#3119);
#2942=LINE('',#7307,#3120);
#2943=LINE('',#7321,#3121);
#2944=LINE('',#7324,#3122);
#2945=LINE('',#7325,#3123);
#2946=LINE('',#7337,#3124);
#2947=LINE('',#7342,#3125);
#2948=LINE('',#7346,#3126);
#2949=LINE('',#7349,#3127);
#2950=LINE('',#7351,#3128);
#2951=LINE('',#7353,#3129);
#2952=LINE('',#7355,#3130);
#2953=LINE('',#7368,#3131);
#2954=LINE('',#7371,#3132);
#2955=LINE('',#7372,#3133);
#2956=LINE('',#7394,#3134);
#2957=LINE('',#7399,#3135);
#2958=LINE('',#7429,#3136);
#2959=LINE('',#7475,#3137);
#2960=LINE('',#8030,#3138);
#2961=LINE('',#8033,#3139);
#2962=LINE('',#8035,#3140);
#2963=LINE('',#8037,#3141);
#2964=LINE('',#8043,#3142);
#2965=LINE('',#8047,#3143);
#2966=LINE('',#8051,#3144);
#2967=LINE('',#8053,#3145);
#2968=LINE('',#8077,#3146);
#2969=LINE('',#8082,#3147);
#2970=LINE('',#8091,#3148);
#2971=LINE('',#8096,#3149);
#2972=LINE('',#8098,#3150);
#2973=LINE('',#8099,#3151);
#2974=LINE('',#8101,#3152);
#2975=LINE('',#8117,#3153);
#2976=LINE('',#8118,#3154);
#2977=LINE('',#8122,#3155);
#2978=LINE('',#8124,#3156);
#2979=LINE('',#8156,#3157);
#2980=LINE('',#8158,#3158);
#2981=LINE('',#8162,#3159);
#2982=LINE('',#8169,#3160);
#2983=LINE('',#8196,#3161);
#2984=LINE('',#8209,#3162);
#2985=LINE('',#8240,#3163);
#2986=LINE('',#8355,#3164);
#2987=LINE('',#8360,#3165);
#2988=LINE('',#8362,#3166);
#2989=LINE('',#8363,#3167);
#2990=LINE('',#8377,#3168);
#2991=LINE('',#8379,#3169);
#2992=LINE('',#8388,#3170);
#2993=LINE('',#8396,#3171);
#2994=LINE('',#8397,#3172);
#2995=LINE('',#8399,#3173);
#2996=LINE('',#8431,#3174);
#2997=LINE('',#8439,#3175);
#2998=LINE('',#8441,#3176);
#2999=LINE('',#8445,#3177);
#3000=LINE('',#8447,#3178);
#3001=LINE('',#8452,#3179);
#3002=LINE('',#8460,#3180);
#3003=LINE('',#8499,#3181);
#3004=LINE('',#8507,#3182);
#3005=LINE('',#8512,#3183);
#3006=LINE('',#8516,#3184);
#3007=LINE('',#8520,#3185);
#3008=LINE('',#8525,#3186);
#3009=LINE('',#8526,#3187);
#3010=LINE('',#8528,#3188);
#3011=LINE('',#8529,#3189);
#3012=VECTOR('',#5068,1.);
#3013=VECTOR('',#5069,1.);
#3014=VECTOR('',#5070,1.);
#3015=VECTOR('',#5073,1.);
#3016=VECTOR('',#5074,1.);
#3017=VECTOR('',#5077,1.);
#3018=VECTOR('',#5078,1.);
#3019=VECTOR('',#5081,1.);
#3020=VECTOR('',#5082,1.);
#3021=VECTOR('',#5085,1.);
#3022=VECTOR('',#5086,1.);
#3023=VECTOR('',#5089,1.);
#3024=VECTOR('',#5158,1.);
#3025=VECTOR('',#5161,1.);
#3026=VECTOR('',#5164,1.);
#3027=VECTOR('',#5165,1.);
#3028=VECTOR('',#5166,1.);
#3029=VECTOR('',#5171,1.);
#3030=VECTOR('',#5176,1.);
#3031=VECTOR('',#5177,1.);
#3032=VECTOR('',#5312,1.);
#3033=VECTOR('',#5315,1.);
#3034=VECTOR('',#5330,1.);
#3035=VECTOR('',#5331,1.);
#3036=VECTOR('',#5336,1.);
#3037=VECTOR('',#5337,1.);
#3038=VECTOR('',#5340,1.);
#3039=VECTOR('',#5343,1.);
#3040=VECTOR('',#5346,1.);
#3041=VECTOR('',#5349,1.);
#3042=VECTOR('',#5354,1.);
#3043=VECTOR('',#5355,1.);
#3044=VECTOR('',#5360,1.);
#3045=VECTOR('',#5361,1.);
#3046=VECTOR('',#5364,1.);
#3047=VECTOR('',#5365,1.);
#3048=VECTOR('',#5368,1.);
#3049=VECTOR('',#5371,1.);
#3050=VECTOR('',#5382,1.);
#3051=VECTOR('',#5383,1.);
#3052=VECTOR('',#5392,1.);
#3053=VECTOR('',#5395,1.);
#3054=VECTOR('',#5400,1.);
#3055=VECTOR('',#5401,1.);
#3056=VECTOR('',#5404,1.);
#3057=VECTOR('',#5405,1.);
#3058=VECTOR('',#5410,1.);
#3059=VECTOR('',#5411,1.);
#3060=VECTOR('',#5416,1.);
#3061=VECTOR('',#5417,1.);
#3062=VECTOR('',#5420,1.);
#3063=VECTOR('',#5421,1.);
#3064=VECTOR('',#5424,1.);
#3065=VECTOR('',#5425,1.);
#3066=VECTOR('',#5428,1.);
#3067=VECTOR('',#5429,1.);
#3068=VECTOR('',#5456,1.);
#3069=VECTOR('',#5457,1.);
#3070=VECTOR('',#5460,1.);
#3071=VECTOR('',#5461,1.);
#3072=VECTOR('',#5470,1.);
#3073=VECTOR('',#5471,1.);
#3074=VECTOR('',#5478,1.);
#3075=VECTOR('',#5479,1.);
#3076=VECTOR('',#5484,1.);
#3077=VECTOR('',#5485,1.);
#3078=VECTOR('',#5486,1.);
#3079=VECTOR('',#5487,1.);
#3080=VECTOR('',#5490,1.);
#3081=VECTOR('',#5491,1.);
#3082=VECTOR('',#5492,1.);
#3083=VECTOR('',#5493,1.);
#3084=VECTOR('',#5496,1.);
#3085=VECTOR('',#5499,1.);
#3086=VECTOR('',#5512,1.);
#3087=VECTOR('',#5515,1.);
#3088=VECTOR('',#5520,1.);
#3089=VECTOR('',#5521,1.);
#3090=VECTOR('',#5526,1.);
#3091=VECTOR('',#5529,1.);
#3092=VECTOR('',#5532,1.);
#3093=VECTOR('',#5533,1.);
#3094=VECTOR('',#5564,1.);
#3095=VECTOR('',#5571,1.);
#3096=VECTOR('',#5580,1.);
#3097=VECTOR('',#5587,1.);
#3098=VECTOR('',#5600,1.);
#3099=VECTOR('',#5611,1.);
#3100=VECTOR('',#5616,1.);
#3101=VECTOR('',#5625,1.);
#3102=VECTOR('',#5630,1.);
#3103=VECTOR('',#5639,1.);
#3104=VECTOR('',#5650,1.);
#3105=VECTOR('',#5657,1.);
#3106=VECTOR('',#5666,1.);
#3107=VECTOR('',#5673,1.);
#3108=VECTOR('',#5684,1.);
#3109=VECTOR('',#5689,1.);
#3110=VECTOR('',#5702,1.);
#3111=VECTOR('',#5707,1.);
#3112=VECTOR('',#5712,1.);
#3113=VECTOR('',#5713,1.);
#3114=VECTOR('',#5716,1.);
#3115=VECTOR('',#5717,1.);
#3116=VECTOR('',#5726,1.);
#3117=VECTOR('',#5727,1.);
#3118=VECTOR('',#5728,1.);
#3119=VECTOR('',#5729,1.);
#3120=VECTOR('',#5736,1.);
#3121=VECTOR('',#5741,1.);
#3122=VECTOR('',#5742,1.);
#3123=VECTOR('',#5743,1.);
#3124=VECTOR('',#5754,1.);
#3125=VECTOR('',#5757,1.);
#3126=VECTOR('',#5762,1.);
#3127=VECTOR('',#5763,1.);
#3128=VECTOR('',#5764,1.);
#3129=VECTOR('',#5765,1.);
#3130=VECTOR('',#5768,1.);
#3131=VECTOR('',#5777,1.);
#3132=VECTOR('',#5778,1.);
#3133=VECTOR('',#5779,1.);
#3134=VECTOR('',#5790,1.);
#3135=VECTOR('',#5793,1.);
#3136=VECTOR('',#5802,1.);
#3137=VECTOR('',#5813,1.);
#3138=VECTOR('',#6106,1.);
#3139=VECTOR('',#6107,1.);
#3140=VECTOR('',#6108,1.);
#3141=VECTOR('',#6109,1.);
#3142=VECTOR('',#6116,1.);
#3143=VECTOR('',#6121,1.);
#3144=VECTOR('',#6126,1.);
#3145=VECTOR('',#6129,1.);
#3146=VECTOR('',#6162,1.);
#3147=VECTOR('',#6165,1.);
#3148=VECTOR('',#6176,1.);
#3149=VECTOR('',#6179,1.);
#3150=VECTOR('',#6180,1.);
#3151=VECTOR('',#6181,1.);
#3152=VECTOR('',#6184,1.);
#3153=VECTOR('',#6185,1.);
#3154=VECTOR('',#6186,1.);
#3155=VECTOR('',#6189,1.);
#3156=VECTOR('',#6192,1.);
#3157=VECTOR('',#6195,1.);
#3158=VECTOR('',#6196,1.);
#3159=VECTOR('',#6199,1.);
#3160=VECTOR('',#6202,1.);
#3161=VECTOR('',#6211,1.);
#3162=VECTOR('',#6222,1.);
#3163=VECTOR('',#6229,1.);
#3164=VECTOR('',#6284,1.);
#3165=VECTOR('',#6287,1.);
#3166=VECTOR('',#6288,1.);
#3167=VECTOR('',#6289,1.);
#3168=VECTOR('',#6308,1.);
#3169=VECTOR('',#6309,1.);
#3170=VECTOR('',#6310,1.);
#3171=VECTOR('',#6311,1.);
#3172=VECTOR('',#6312,1.);
#3173=VECTOR('',#6315,1.);
#3174=VECTOR('',#6318,1.);
#3175=VECTOR('',#6319,1.);
#3176=VECTOR('',#6320,1.);
#3177=VECTOR('',#6323,1.);
#3178=VECTOR('',#6326,1.);
#3179=VECTOR('',#6333,1.);
#3180=VECTOR('',#6344,1.);
#3181=VECTOR('',#6357,1.);
#3182=VECTOR('',#6372,1.);
#3183=VECTOR('',#6375,1.);
#3184=VECTOR('',#6380,1.);
#3185=VECTOR('',#6383,1.);
#3186=VECTOR('',#6388,1.);
#3187=VECTOR('',#6389,1.);
#3188=VECTOR('',#6392,1.);
#3189=VECTOR('',#6393,1.);
#3190=EDGE_LOOP('',(#699,#700,#701,#702,#703));
#3191=EDGE_LOOP('',(#704,#705,#706,#707,#708));
#3192=EDGE_LOOP('',(#709,#710,#711,#712,#713));
#3193=EDGE_LOOP('',(#714,#715,#716,#717,#718));
#3194=EDGE_LOOP('',(#719,#720,#721,#722,#723));
#3195=EDGE_LOOP('',(#724,#725,#726,#727,#728));
#3196=EDGE_LOOP('',(#729));
#3197=EDGE_LOOP('',(#730,#731,#732,#733,#734,#735));
#3198=EDGE_LOOP('',(#736));
#3199=EDGE_LOOP('',(#737));
#3200=EDGE_LOOP('',(#738));
#3201=EDGE_LOOP('',(#739,#740,#741));
#3202=EDGE_LOOP('',(#742,#743,#744));
#3203=EDGE_LOOP('',(#745,#746,#747));
#3204=EDGE_LOOP('',(#748,#749,#750));
#3205=EDGE_LOOP('',(#751,#752,#753));
#3206=EDGE_LOOP('',(#754,#755,#756));
#3207=EDGE_LOOP('',(#757,#758,#759,#760,#761,#762));
#3208=EDGE_LOOP('',(#763));
#3209=EDGE_LOOP('',(#764));
#3210=EDGE_LOOP('',(#765));
#3211=EDGE_LOOP('',(#766));
#3212=EDGE_LOOP('',(#767));
#3213=EDGE_LOOP('',(#768));
#3214=EDGE_LOOP('',(#769));
#3215=EDGE_LOOP('',(#770));
#3216=EDGE_LOOP('',(#771));
#3217=EDGE_LOOP('',(#772));
#3218=EDGE_LOOP('',(#773));
#3219=EDGE_LOOP('',(#774));
#3220=EDGE_LOOP('',(#775,#776,#777,#778));
#3221=EDGE_LOOP('',(#779,#780,#781,#782));
#3222=EDGE_LOOP('',(#783,#784,#785,#786));
#3223=EDGE_LOOP('',(#787,#788,#789,#790));
#3224=EDGE_LOOP('',(#791,#792,#793,#794));
#3225=EDGE_LOOP('',(#795,#796,#797,#798));
#3226=EDGE_LOOP('',(#799));
#3227=EDGE_LOOP('',(#800));
#3228=EDGE_LOOP('',(#801));
#3229=EDGE_LOOP('',(#802));
#3230=EDGE_LOOP('',(#803));
#3231=EDGE_LOOP('',(#804));
#3232=EDGE_LOOP('',(#805));
#3233=EDGE_LOOP('',(#806));
#3234=EDGE_LOOP('',(#807));
#3235=EDGE_LOOP('',(#808));
#3236=EDGE_LOOP('',(#809));
#3237=EDGE_LOOP('',(#810));
#3238=EDGE_LOOP('',(#811));
#3239=EDGE_LOOP('',(#812));
#3240=EDGE_LOOP('',(#813));
#3241=EDGE_LOOP('',(#814));
#3242=EDGE_LOOP('',(#815));
#3243=EDGE_LOOP('',(#816));
#3244=EDGE_LOOP('',(#817));
#3245=EDGE_LOOP('',(#818));
#3246=EDGE_LOOP('',(#819));
#3247=EDGE_LOOP('',(#820));
#3248=EDGE_LOOP('',(#821));
#3249=EDGE_LOOP('',(#822));
#3250=EDGE_LOOP('',(#823));
#3251=EDGE_LOOP('',(#824));
#3252=EDGE_LOOP('',(#825));
#3253=EDGE_LOOP('',(#826));
#3254=EDGE_LOOP('',(#827));
#3255=EDGE_LOOP('',(#828));
#3256=EDGE_LOOP('',(#829));
#3257=EDGE_LOOP('',(#830));
#3258=EDGE_LOOP('',(#831));
#3259=EDGE_LOOP('',(#832));
#3260=EDGE_LOOP('',(#833));
#3261=EDGE_LOOP('',(#834));
#3262=EDGE_LOOP('',(#835));
#3263=EDGE_LOOP('',(#836));
#3264=EDGE_LOOP('',(#837));
#3265=EDGE_LOOP('',(#838));
#3266=EDGE_LOOP('',(#839));
#3267=EDGE_LOOP('',(#840));
#3268=EDGE_LOOP('',(#841));
#3269=EDGE_LOOP('',(#842));
#3270=EDGE_LOOP('',(#843));
#3271=EDGE_LOOP('',(#844));
#3272=EDGE_LOOP('',(#845));
#3273=EDGE_LOOP('',(#846));
#3274=EDGE_LOOP('',(#847));
#3275=EDGE_LOOP('',(#848));
#3276=EDGE_LOOP('',(#849));
#3277=EDGE_LOOP('',(#850));
#3278=EDGE_LOOP('',(#851));
#3279=EDGE_LOOP('',(#852));
#3280=EDGE_LOOP('',(#853));
#3281=EDGE_LOOP('',(#854));
#3282=EDGE_LOOP('',(#855));
#3283=EDGE_LOOP('',(#856));
#3284=EDGE_LOOP('',(#857));
#3285=EDGE_LOOP('',(#858));
#3286=EDGE_LOOP('',(#859));
#3287=EDGE_LOOP('',(#860));
#3288=EDGE_LOOP('',(#861));
#3289=EDGE_LOOP('',(#862));
#3290=EDGE_LOOP('',(#863,#864,#865,#866));
#3291=EDGE_LOOP('',(#867,#868,#869,#870));
#3292=EDGE_LOOP('',(#871,#872,#873,#874));
#3293=EDGE_LOOP('',(#875,#876,#877,#878));
#3294=EDGE_LOOP('',(#879,#880,#881,#882));
#3295=EDGE_LOOP('',(#883,#884,#885,#886));
#3296=EDGE_LOOP('',(#887,#888,#889,#890));
#3297=EDGE_LOOP('',(#891,#892,#893,#894));
#3298=EDGE_LOOP('',(#895,#896,#897,#898));
#3299=EDGE_LOOP('',(#899,#900,#901,#902));
#3300=EDGE_LOOP('',(#903,#904,#905,#906));
#3301=EDGE_LOOP('',(#907,#908,#909,#910));
#3302=EDGE_LOOP('',(#911,#912,#913,#914));
#3303=EDGE_LOOP('',(#915,#916,#917,#918));
#3304=EDGE_LOOP('',(#919,#920,#921,#922));
#3305=EDGE_LOOP('',(#923,#924,#925,#926));
#3306=EDGE_LOOP('',(#927,#928,#929,#930));
#3307=EDGE_LOOP('',(#931,#932,#933,#934));
#3308=EDGE_LOOP('',(#935,#936,#937,#938));
#3309=EDGE_LOOP('',(#939,#940,#941,#942));
#3310=EDGE_LOOP('',(#943,#944,#945,#946,#947,#948,#949,#950));
#3311=EDGE_LOOP('',(#951,#952,#953,#954,#955,#956,#957,#958));
#3312=EDGE_LOOP('',(#959));
#3313=EDGE_LOOP('',(#960,#961,#962,#963));
#3314=EDGE_LOOP('',(#964));
#3315=EDGE_LOOP('',(#965));
#3316=EDGE_LOOP('',(#966));
#3317=EDGE_LOOP('',(#967,#968,#969,#970));
#3318=EDGE_LOOP('',(#971));
#3319=EDGE_LOOP('',(#972));
#3320=EDGE_LOOP('',(#973,#974,#975,#976,#977,#978,#979,#980,#981,#982,#983,
#984));
#3321=EDGE_LOOP('',(#985));
#3322=EDGE_LOOP('',(#986,#987,#988,#989,#990,#991,#992,#993,#994,#995,#996,
#997));
#3323=EDGE_LOOP('',(#998));
#3324=EDGE_LOOP('',(#999,#1000,#1001,#1002,#1003,#1004,#1005,#1006));
#3325=EDGE_LOOP('',(#1007,#1008,#1009,#1010,#1011,#1012,#1013,#1014));
#3326=EDGE_LOOP('',(#1015,#1016,#1017,#1018));
#3327=EDGE_LOOP('',(#1019,#1020,#1021,#1022));
#3328=EDGE_LOOP('',(#1023,#1024,#1025,#1026));
#3329=EDGE_LOOP('',(#1027));
#3330=EDGE_LOOP('',(#1028));
#3331=EDGE_LOOP('',(#1029));
#3332=EDGE_LOOP('',(#1030));
#3333=EDGE_LOOP('',(#1031,#1032,#1033,#1034));
#3334=EDGE_LOOP('',(#1035,#1036,#1037,#1038));
#3335=EDGE_LOOP('',(#1039,#1040,#1041,#1042));
#3336=EDGE_LOOP('',(#1043,#1044,#1045,#1046));
#3337=EDGE_LOOP('',(#1047,#1048,#1049,#1050));
#3338=EDGE_LOOP('',(#1051,#1052,#1053,#1054));
#3339=EDGE_LOOP('',(#1055,#1056,#1057,#1058));
#3340=EDGE_LOOP('',(#1059,#1060,#1061,#1062));
#3341=EDGE_LOOP('',(#1063,#1064,#1065,#1066));
#3342=EDGE_LOOP('',(#1067,#1068,#1069,#1070));
#3343=EDGE_LOOP('',(#1071,#1072,#1073,#1074,#1075,#1076,#1077,#1078));
#3344=EDGE_LOOP('',(#1079,#1080,#1081,#1082,#1083,#1084,#1085,#1086));
#3345=EDGE_LOOP('',(#1087,#1088,#1089,#1090,#1091,#1092));
#3346=EDGE_LOOP('',(#1093));
#3347=EDGE_LOOP('',(#1094,#1095,#1096,#1097,#1098,#1099,#1100,#1101));
#3348=EDGE_LOOP('',(#1102,#1103,#1104,#1105,#1106,#1107,#1108,#1109));
#3349=EDGE_LOOP('',(#1110,#1111,#1112,#1113,#1114,#1115));
#3350=EDGE_LOOP('',(#1116));
#3351=EDGE_LOOP('',(#1117,#1118,#1119,#1120,#1121,#1122,#1123,#1124));
#3352=EDGE_LOOP('',(#1125,#1126,#1127,#1128,#1129,#1130,#1131,#1132));
#3353=EDGE_LOOP('',(#1133));
#3354=EDGE_LOOP('',(#1134,#1135,#1136,#1137,#1138,#1139,#1140,#1141));
#3355=EDGE_LOOP('',(#1142,#1143,#1144,#1145));
#3356=EDGE_LOOP('',(#1146));
#3357=EDGE_LOOP('',(#1147,#1148,#1149,#1150,#1151,#1152,#1153,#1154));
#3358=EDGE_LOOP('',(#1155,#1156,#1157,#1158));
#3359=EDGE_LOOP('',(#1159,#1160,#1161,#1162));
#3360=EDGE_LOOP('',(#1163));
#3361=EDGE_LOOP('',(#1164));
#3362=EDGE_LOOP('',(#1165,#1166,#1167,#1168));
#3363=EDGE_LOOP('',(#1169,#1170,#1171,#1172,#1173,#1174,#1175,#1176));
#3364=EDGE_LOOP('',(#1177,#1178,#1179,#1180));
#3365=EDGE_LOOP('',(#1181,#1182,#1183,#1184,#1185,#1186));
#3366=EDGE_LOOP('',(#1187,#1188,#1189,#1190));
#3367=EDGE_LOOP('',(#1191,#1192,#1193,#1194));
#3368=EDGE_LOOP('',(#1195,#1196,#1197,#1198,#1199,#1200));
#3369=EDGE_LOOP('',(#1201,#1202,#1203,#1204));
#3370=EDGE_LOOP('',(#1205,#1206,#1207,#1208,#1209,#1210,#1211,#1212));
#3371=EDGE_LOOP('',(#1213,#1214,#1215,#1216));
#3372=EDGE_LOOP('',(#1217,#1218,#1219,#1220,#1221));
#3373=EDGE_LOOP('',(#1222,#1223,#1224,#1225));
#3374=EDGE_LOOP('',(#1226,#1227,#1228,#1229,#1230));
#3375=EDGE_LOOP('',(#1231,#1232,#1233,#1234,#1235));
#3376=EDGE_LOOP('',(#1236,#1237,#1238,#1239));
#3377=EDGE_LOOP('',(#1240,#1241,#1242,#1243,#1244));
#3378=EDGE_LOOP('',(#1245,#1246,#1247,#1248,#1249,#1250));
#3379=EDGE_LOOP('',(#1251,#1252,#1253,#1254,#1255,#1256));
#3380=EDGE_LOOP('',(#1257,#1258,#1259,#1260));
#3381=EDGE_LOOP('',(#1261,#1262,#1263,#1264));
#3382=EDGE_LOOP('',(#1265,#1266,#1267,#1268));
#3383=EDGE_LOOP('',(#1269,#1270,#1271,#1272));
#3384=EDGE_LOOP('',(#1273));
#3385=EDGE_LOOP('',(#1274));
#3386=EDGE_LOOP('',(#1275));
#3387=EDGE_LOOP('',(#1276));
#3388=EDGE_LOOP('',(#1277,#1278,#1279,#1280));
#3389=EDGE_LOOP('',(#1281,#1282,#1283,#1284));
#3390=EDGE_LOOP('',(#1285,#1286,#1287,#1288));
#3391=EDGE_LOOP('',(#1289,#1290,#1291,#1292));
#3392=EDGE_LOOP('',(#1293,#1294,#1295,#1296));
#3393=EDGE_LOOP('',(#1297,#1298,#1299,#1300));
#3394=EDGE_LOOP('',(#1301,#1302,#1303,#1304));
#3395=EDGE_LOOP('',(#1305,#1306,#1307,#1308));
#3396=EDGE_LOOP('',(#1309,#1310,#1311,#1312));
#3397=EDGE_LOOP('',(#1313,#1314,#1315,#1316));
#3398=EDGE_LOOP('',(#1317,#1318,#1319,#1320));
#3399=EDGE_LOOP('',(#1321,#1322,#1323,#1324));
#3400=EDGE_LOOP('',(#1325,#1326,#1327,#1328));
#3401=EDGE_LOOP('',(#1329,#1330,#1331,#1332));
#3402=EDGE_LOOP('',(#1333,#1334,#1335,#1336));
#3403=EDGE_LOOP('',(#1337,#1338,#1339,#1340));
#3404=EDGE_LOOP('',(#1341,#1342,#1343,#1344));
#3405=EDGE_LOOP('',(#1345,#1346,#1347,#1348));
#3406=EDGE_LOOP('',(#1349,#1350,#1351,#1352));
#3407=EDGE_LOOP('',(#1353,#1354,#1355,#1356));
#3408=EDGE_LOOP('',(#1357,#1358,#1359,#1360));
#3409=EDGE_LOOP('',(#1361,#1362,#1363,#1364));
#3410=EDGE_LOOP('',(#1365,#1366,#1367,#1368));
#3411=EDGE_LOOP('',(#1369,#1370,#1371,#1372));
#3412=EDGE_LOOP('',(#1373,#1374,#1375,#1376));
#3413=EDGE_LOOP('',(#1377,#1378,#1379,#1380));
#3414=EDGE_LOOP('',(#1381,#1382,#1383,#1384));
#3415=EDGE_LOOP('',(#1385,#1386,#1387,#1388));
#3416=EDGE_LOOP('',(#1389,#1390,#1391,#1392));
#3417=EDGE_LOOP('',(#1393,#1394,#1395,#1396));
#3418=EDGE_LOOP('',(#1397,#1398,#1399,#1400));
#3419=EDGE_LOOP('',(#1401,#1402,#1403,#1404));
#3420=EDGE_LOOP('',(#1405,#1406,#1407,#1408));
#3421=EDGE_LOOP('',(#1409,#1410,#1411,#1412));
#3422=EDGE_LOOP('',(#1413,#1414,#1415,#1416));
#3423=EDGE_LOOP('',(#1417,#1418,#1419,#1420));
#3424=EDGE_LOOP('',(#1421,#1422,#1423,#1424));
#3425=EDGE_LOOP('',(#1425,#1426,#1427,#1428));
#3426=EDGE_LOOP('',(#1429,#1430,#1431,#1432));
#3427=EDGE_LOOP('',(#1433,#1434,#1435,#1436));
#3428=EDGE_LOOP('',(#1437,#1438,#1439,#1440));
#3429=EDGE_LOOP('',(#1441,#1442,#1443,#1444));
#3430=EDGE_LOOP('',(#1445,#1446,#1447,#1448));
#3431=EDGE_LOOP('',(#1449,#1450,#1451,#1452));
#3432=EDGE_LOOP('',(#1453,#1454,#1455,#1456));
#3433=EDGE_LOOP('',(#1457,#1458,#1459,#1460));
#3434=EDGE_LOOP('',(#1461,#1462,#1463,#1464));
#3435=EDGE_LOOP('',(#1465,#1466,#1467,#1468));
#3436=EDGE_LOOP('',(#1469,#1470,#1471));
#3437=EDGE_LOOP('',(#1472,#1473,#1474,#1475));
#3438=EDGE_LOOP('',(#1476,#1477,#1478));
#3439=EDGE_LOOP('',(#1479,#1480,#1481));
#3440=EDGE_LOOP('',(#1482,#1483,#1484,#1485));
#3441=EDGE_LOOP('',(#1486,#1487,#1488));
#3442=EDGE_LOOP('',(#1489,#1490,#1491));
#3443=EDGE_LOOP('',(#1492,#1493,#1494,#1495));
#3444=EDGE_LOOP('',(#1496,#1497,#1498));
#3445=EDGE_LOOP('',(#1499,#1500,#1501));
#3446=EDGE_LOOP('',(#1502,#1503,#1504,#1505));
#3447=EDGE_LOOP('',(#1506,#1507,#1508));
#3448=EDGE_LOOP('',(#1509,#1510,#1511,#1512));
#3449=EDGE_LOOP('',(#1513,#1514,#1515,#1516));
#3450=EDGE_LOOP('',(#1517,#1518,#1519,#1520));
#3451=EDGE_LOOP('',(#1521,#1522,#1523));
#3452=EDGE_LOOP('',(#1524,#1525,#1526));
#3453=EDGE_LOOP('',(#1527,#1528,#1529,#1530));
#3454=EDGE_LOOP('',(#1531,#1532,#1533,#1534));
#3455=EDGE_LOOP('',(#1535,#1536,#1537,#1538));
#3456=EDGE_LOOP('',(#1539));
#3457=EDGE_LOOP('',(#1540));
#3458=EDGE_LOOP('',(#1541));
#3459=EDGE_LOOP('',(#1542));
#3460=EDGE_LOOP('',(#1543));
#3461=EDGE_LOOP('',(#1544));
#3462=EDGE_LOOP('',(#1545,#1546,#1547,#1548));
#3463=EDGE_LOOP('',(#1549,#1550,#1551,#1552));
#3464=EDGE_LOOP('',(#1553,#1554,#1555,#1556));
#3465=EDGE_LOOP('',(#1557,#1558,#1559));
#3466=EDGE_LOOP('',(#1560,#1561,#1562));
#3467=EDGE_LOOP('',(#1563,#1564,#1565,#1566));
#3468=EDGE_LOOP('',(#1567,#1568,#1569,#1570));
#3469=EDGE_LOOP('',(#1571,#1572,#1573,#1574));
#3470=EDGE_LOOP('',(#1575));
#3471=EDGE_LOOP('',(#1576));
#3472=EDGE_LOOP('',(#1577,#1578,#1579,#1580,#1581,#1582,#1583,#1584,#1585,
#1586,#1587,#1588));
#3473=EDGE_LOOP('',(#1589));
#3474=EDGE_LOOP('',(#1590,#1591,#1592,#1593,#1594,#1595,#1596,#1597,#1598,
#1599,#1600,#1601));
#3475=EDGE_LOOP('',(#1602));
#3476=EDGE_LOOP('',(#1603,#1604,#1605,#1606));
#3477=EDGE_LOOP('',(#1607,#1608,#1609,#1610));
#3478=EDGE_LOOP('',(#1611,#1612,#1613,#1614));
#3479=EDGE_LOOP('',(#1615,#1616,#1617,#1618));
#3480=EDGE_LOOP('',(#1619,#1620,#1621,#1622));
#3481=EDGE_LOOP('',(#1623,#1624,#1625,#1626));
#3482=EDGE_LOOP('',(#1627));
#3483=EDGE_LOOP('',(#1628));
#3484=EDGE_LOOP('',(#1629));
#3485=EDGE_LOOP('',(#1630));
#3486=EDGE_LOOP('',(#1631));
#3487=EDGE_LOOP('',(#1632));
#3488=EDGE_LOOP('',(#1633));
#3489=EDGE_LOOP('',(#1634));
#3490=EDGE_LOOP('',(#1635));
#3491=EDGE_LOOP('',(#1636));
#3492=EDGE_LOOP('',(#1637));
#3493=EDGE_LOOP('',(#1638,#1639,#1640,#1641));
#3494=EDGE_LOOP('',(#1642));
#3495=EDGE_LOOP('',(#1643));
#3496=EDGE_LOOP('',(#1644,#1645,#1646,#1647,#1648,#1649));
#3497=EDGE_LOOP('',(#1650,#1651,#1652,#1653,#1654,#1655,#1656,#1657,#1658));
#3498=EDGE_LOOP('',(#1659,#1660,#1661,#1662));
#3499=EDGE_LOOP('',(#1663,#1664,#1665,#1666,#1667,#1668,#1669,#1670,#1671));
#3500=EDGE_LOOP('',(#1672,#1673,#1674,#1675,#1676));
#3501=EDGE_LOOP('',(#1677,#1678));
#3502=EDGE_LOOP('',(#1679));
#3503=EDGE_LOOP('',(#1680));
#3504=EDGE_LOOP('',(#1681,#1682,#1683,#1684));
#3505=EDGE_LOOP('',(#1685,#1686,#1687,#1688,#1689,#1690));
#3506=EDGE_LOOP('',(#1691,#1692,#1693,#1694));
#3507=EDGE_LOOP('',(#1695,#1696,#1697,#1698,#1699,#1700));
#3508=EDGE_LOOP('',(#1701,#1702,#1703,#1704));
#3509=EDGE_LOOP('',(#1705,#1706,#1707,#1708));
#3510=EDGE_LOOP('',(#1709,#1710));
#3511=EDGE_LOOP('',(#1711,#1712));
#3512=EDGE_LOOP('',(#1713,#1714));
#3513=EDGE_LOOP('',(#1715,#1716));
#3514=EDGE_LOOP('',(#1717,#1718,#1719,#1720));
#3515=EDGE_LOOP('',(#1721));
#3516=EDGE_LOOP('',(#1722));
#3517=EDGE_LOOP('',(#1723));
#3518=EDGE_LOOP('',(#1724));
#3519=EDGE_LOOP('',(#1725,#1726,#1727,#1728));
#3520=EDGE_LOOP('',(#1729,#1730,#1731,#1732));
#3521=EDGE_LOOP('',(#1733,#1734,#1735,#1736));
#3522=EDGE_LOOP('',(#1737,#1738,#1739,#1740));
#3523=EDGE_LOOP('',(#1741));
#3524=EDGE_LOOP('',(#1742));
#3525=EDGE_LOOP('',(#1743,#1744,#1745,#1746));
#3526=EDGE_LOOP('',(#1747));
#3527=EDGE_LOOP('',(#1748));
#3528=EDGE_LOOP('',(#1749,#1750,#1751,#1752));
#3529=EDGE_LOOP('',(#1753));
#3530=EDGE_LOOP('',(#1754));
#3531=EDGE_LOOP('',(#1755,#1756,#1757,#1758,#1759,#1760));
#3532=EDGE_LOOP('',(#1761));
#3533=EDGE_LOOP('',(#1762));
#3534=EDGE_LOOP('',(#1763,#1764));
#3535=EDGE_LOOP('',(#1765,#1766));
#3536=EDGE_LOOP('',(#1767));
#3537=EDGE_LOOP('',(#1768,#1769));
#3538=EDGE_LOOP('',(#1770,#1771));
#3539=EDGE_LOOP('',(#1772,#1773,#1774,#1775,#1776,#1777,#1778,#1779,#1780));
#3540=EDGE_LOOP('',(#1781,#1782,#1783,#1784));
#3541=EDGE_LOOP('',(#1785,#1786,#1787,#1788,#1789,#1790,#1791,#1792,#1793));
#3542=EDGE_LOOP('',(#1794,#1795,#1796,#1797,#1798));
#3543=EDGE_LOOP('',(#1799));
#3544=EDGE_LOOP('',(#1800));
#3545=EDGE_LOOP('',(#1801,#1802,#1803,#1804));
#3546=EDGE_LOOP('',(#1805,#1806,#1807,#1808,#1809,#1810));
#3547=EDGE_LOOP('',(#1811,#1812,#1813,#1814));
#3548=EDGE_LOOP('',(#1815,#1816,#1817,#1818,#1819,#1820));
#3549=EDGE_LOOP('',(#1821));
#3550=EDGE_LOOP('',(#1822,#1823,#1824,#1825));
#3551=EDGE_LOOP('',(#1826,#1827,#1828,#1829));
#3552=EDGE_LOOP('',(#1830,#1831,#1832,#1833));
#3553=EDGE_LOOP('',(#1834,#1835,#1836,#1837));
#3554=EDGE_LOOP('',(#1838));
#3555=EDGE_LOOP('',(#1839));
#3556=EDGE_LOOP('',(#1840));
#3557=EDGE_LOOP('',(#1841));
#3558=EDGE_LOOP('',(#1842));
#3559=EDGE_LOOP('',(#1843));
#3560=EDGE_LOOP('',(#1844));
#3561=EDGE_LOOP('',(#1845,#1846,#1847,#1848));
#3562=EDGE_LOOP('',(#1849,#1850,#1851,#1852));
#3563=EDGE_LOOP('',(#1853,#1854,#1855,#1856));
#3564=EDGE_LOOP('',(#1857,#1858,#1859,#1860));
#3565=EDGE_LOOP('',(#1861,#1862,#1863,#1864));
#3566=EDGE_LOOP('',(#1865,#1866,#1867,#1868));
#3567=FACE_BOUND('',#3190,.T.);
#3568=FACE_BOUND('',#3191,.T.);
#3569=FACE_BOUND('',#3192,.T.);
#3570=FACE_BOUND('',#3193,.T.);
#3571=FACE_BOUND('',#3194,.T.);
#3572=FACE_BOUND('',#3195,.T.);
#3573=FACE_BOUND('',#3196,.T.);
#3574=FACE_BOUND('',#3197,.T.);
#3575=FACE_BOUND('',#3198,.T.);
#3576=FACE_BOUND('',#3199,.T.);
#3577=FACE_BOUND('',#3200,.T.);
#3578=FACE_BOUND('',#3201,.T.);
#3579=FACE_BOUND('',#3202,.T.);
#3580=FACE_BOUND('',#3203,.T.);
#3581=FACE_BOUND('',#3204,.T.);
#3582=FACE_BOUND('',#3205,.T.);
#3583=FACE_BOUND('',#3206,.T.);
#3584=FACE_BOUND('',#3207,.T.);
#3585=FACE_BOUND('',#3208,.T.);
#3586=FACE_BOUND('',#3209,.T.);
#3587=FACE_BOUND('',#3210,.T.);
#3588=FACE_BOUND('',#3211,.T.);
#3589=FACE_BOUND('',#3212,.T.);
#3590=FACE_BOUND('',#3213,.T.);
#3591=FACE_BOUND('',#3214,.T.);
#3592=FACE_BOUND('',#3215,.T.);
#3593=FACE_BOUND('',#3216,.T.);
#3594=FACE_BOUND('',#3217,.T.);
#3595=FACE_BOUND('',#3218,.T.);
#3596=FACE_BOUND('',#3219,.T.);
#3597=FACE_BOUND('',#3220,.T.);
#3598=FACE_BOUND('',#3221,.T.);
#3599=FACE_BOUND('',#3222,.T.);
#3600=FACE_BOUND('',#3223,.T.);
#3601=FACE_BOUND('',#3224,.T.);
#3602=FACE_BOUND('',#3225,.T.);
#3603=FACE_BOUND('',#3226,.T.);
#3604=FACE_BOUND('',#3227,.T.);
#3605=FACE_BOUND('',#3228,.T.);
#3606=FACE_BOUND('',#3229,.T.);
#3607=FACE_BOUND('',#3230,.T.);
#3608=FACE_BOUND('',#3231,.T.);
#3609=FACE_BOUND('',#3232,.T.);
#3610=FACE_BOUND('',#3233,.T.);
#3611=FACE_BOUND('',#3234,.T.);
#3612=FACE_BOUND('',#3235,.T.);
#3613=FACE_BOUND('',#3236,.T.);
#3614=FACE_BOUND('',#3237,.T.);
#3615=FACE_BOUND('',#3238,.T.);
#3616=FACE_BOUND('',#3239,.T.);
#3617=FACE_BOUND('',#3240,.T.);
#3618=FACE_BOUND('',#3241,.T.);
#3619=FACE_BOUND('',#3242,.T.);
#3620=FACE_BOUND('',#3243,.T.);
#3621=FACE_BOUND('',#3244,.T.);
#3622=FACE_BOUND('',#3245,.T.);
#3623=FACE_BOUND('',#3246,.T.);
#3624=FACE_BOUND('',#3247,.T.);
#3625=FACE_BOUND('',#3248,.T.);
#3626=FACE_BOUND('',#3249,.T.);
#3627=FACE_BOUND('',#3250,.T.);
#3628=FACE_BOUND('',#3251,.T.);
#3629=FACE_BOUND('',#3252,.T.);
#3630=FACE_BOUND('',#3253,.T.);
#3631=FACE_BOUND('',#3254,.T.);
#3632=FACE_BOUND('',#3255,.T.);
#3633=FACE_BOUND('',#3256,.T.);
#3634=FACE_BOUND('',#3257,.T.);
#3635=FACE_BOUND('',#3258,.T.);
#3636=FACE_BOUND('',#3259,.T.);
#3637=FACE_BOUND('',#3260,.T.);
#3638=FACE_BOUND('',#3261,.T.);
#3639=FACE_BOUND('',#3262,.T.);
#3640=FACE_BOUND('',#3263,.T.);
#3641=FACE_BOUND('',#3264,.T.);
#3642=FACE_BOUND('',#3265,.T.);
#3643=FACE_BOUND('',#3266,.T.);
#3644=FACE_BOUND('',#3267,.T.);
#3645=FACE_BOUND('',#3268,.T.);
#3646=FACE_BOUND('',#3269,.T.);
#3647=FACE_BOUND('',#3270,.T.);
#3648=FACE_BOUND('',#3271,.T.);
#3649=FACE_BOUND('',#3272,.T.);
#3650=FACE_BOUND('',#3273,.T.);
#3651=FACE_BOUND('',#3274,.T.);
#3652=FACE_BOUND('',#3275,.T.);
#3653=FACE_BOUND('',#3276,.T.);
#3654=FACE_BOUND('',#3277,.T.);
#3655=FACE_BOUND('',#3278,.T.);
#3656=FACE_BOUND('',#3279,.T.);
#3657=FACE_BOUND('',#3280,.T.);
#3658=FACE_BOUND('',#3281,.T.);
#3659=FACE_BOUND('',#3282,.T.);
#3660=FACE_BOUND('',#3283,.T.);
#3661=FACE_BOUND('',#3284,.T.);
#3662=FACE_BOUND('',#3285,.T.);
#3663=FACE_BOUND('',#3286,.T.);
#3664=FACE_BOUND('',#3287,.T.);
#3665=FACE_BOUND('',#3288,.T.);
#3666=FACE_BOUND('',#3289,.T.);
#3667=FACE_BOUND('',#3290,.T.);
#3668=FACE_BOUND('',#3291,.T.);
#3669=FACE_BOUND('',#3292,.T.);
#3670=FACE_BOUND('',#3293,.T.);
#3671=FACE_BOUND('',#3294,.T.);
#3672=FACE_BOUND('',#3295,.T.);
#3673=FACE_BOUND('',#3296,.T.);
#3674=FACE_BOUND('',#3297,.T.);
#3675=FACE_BOUND('',#3298,.T.);
#3676=FACE_BOUND('',#3299,.T.);
#3677=FACE_BOUND('',#3300,.T.);
#3678=FACE_BOUND('',#3301,.T.);
#3679=FACE_BOUND('',#3302,.T.);
#3680=FACE_BOUND('',#3303,.T.);
#3681=FACE_BOUND('',#3304,.T.);
#3682=FACE_BOUND('',#3305,.T.);
#3683=FACE_BOUND('',#3306,.T.);
#3684=FACE_BOUND('',#3307,.T.);
#3685=FACE_BOUND('',#3308,.T.);
#3686=FACE_BOUND('',#3309,.T.);
#3687=FACE_BOUND('',#3310,.T.);
#3688=FACE_BOUND('',#3311,.T.);
#3689=FACE_BOUND('',#3312,.T.);
#3690=FACE_BOUND('',#3313,.T.);
#3691=FACE_BOUND('',#3314,.T.);
#3692=FACE_BOUND('',#3315,.T.);
#3693=FACE_BOUND('',#3316,.T.);
#3694=FACE_BOUND('',#3317,.T.);
#3695=FACE_BOUND('',#3318,.T.);
#3696=FACE_BOUND('',#3319,.T.);
#3697=FACE_BOUND('',#3320,.T.);
#3698=FACE_BOUND('',#3321,.T.);
#3699=FACE_BOUND('',#3322,.T.);
#3700=FACE_BOUND('',#3323,.T.);
#3701=FACE_BOUND('',#3324,.T.);
#3702=FACE_BOUND('',#3325,.T.);
#3703=FACE_BOUND('',#3326,.T.);
#3704=FACE_BOUND('',#3327,.T.);
#3705=FACE_BOUND('',#3328,.T.);
#3706=FACE_BOUND('',#3329,.T.);
#3707=FACE_BOUND('',#3330,.T.);
#3708=FACE_BOUND('',#3331,.T.);
#3709=FACE_BOUND('',#3332,.T.);
#3710=FACE_BOUND('',#3333,.T.);
#3711=FACE_BOUND('',#3334,.T.);
#3712=FACE_BOUND('',#3335,.T.);
#3713=FACE_BOUND('',#3336,.T.);
#3714=FACE_BOUND('',#3337,.T.);
#3715=FACE_BOUND('',#3338,.T.);
#3716=FACE_BOUND('',#3339,.T.);
#3717=FACE_BOUND('',#3340,.T.);
#3718=FACE_BOUND('',#3341,.T.);
#3719=FACE_BOUND('',#3342,.T.);
#3720=FACE_BOUND('',#3343,.T.);
#3721=FACE_BOUND('',#3344,.T.);
#3722=FACE_BOUND('',#3345,.T.);
#3723=FACE_BOUND('',#3346,.T.);
#3724=FACE_BOUND('',#3347,.T.);
#3725=FACE_BOUND('',#3348,.T.);
#3726=FACE_BOUND('',#3349,.T.);
#3727=FACE_BOUND('',#3350,.T.);
#3728=FACE_BOUND('',#3351,.T.);
#3729=FACE_BOUND('',#3352,.T.);
#3730=FACE_BOUND('',#3353,.T.);
#3731=FACE_BOUND('',#3354,.T.);
#3732=FACE_BOUND('',#3355,.T.);
#3733=FACE_BOUND('',#3356,.T.);
#3734=FACE_BOUND('',#3357,.T.);
#3735=FACE_BOUND('',#3358,.T.);
#3736=FACE_BOUND('',#3359,.T.);
#3737=FACE_BOUND('',#3360,.T.);
#3738=FACE_BOUND('',#3361,.T.);
#3739=FACE_BOUND('',#3362,.T.);
#3740=FACE_BOUND('',#3363,.T.);
#3741=FACE_BOUND('',#3364,.T.);
#3742=FACE_BOUND('',#3365,.T.);
#3743=FACE_BOUND('',#3366,.T.);
#3744=FACE_BOUND('',#3367,.T.);
#3745=FACE_BOUND('',#3368,.T.);
#3746=FACE_BOUND('',#3369,.T.);
#3747=FACE_BOUND('',#3370,.T.);
#3748=FACE_BOUND('',#3371,.T.);
#3749=FACE_BOUND('',#3372,.T.);
#3750=FACE_BOUND('',#3373,.T.);
#3751=FACE_BOUND('',#3374,.T.);
#3752=FACE_BOUND('',#3375,.T.);
#3753=FACE_BOUND('',#3376,.T.);
#3754=FACE_BOUND('',#3377,.T.);
#3755=FACE_BOUND('',#3378,.T.);
#3756=FACE_BOUND('',#3379,.T.);
#3757=FACE_BOUND('',#3380,.T.);
#3758=FACE_BOUND('',#3381,.T.);
#3759=FACE_BOUND('',#3382,.T.);
#3760=FACE_BOUND('',#3383,.T.);
#3761=FACE_BOUND('',#3384,.T.);
#3762=FACE_BOUND('',#3385,.T.);
#3763=FACE_BOUND('',#3386,.T.);
#3764=FACE_BOUND('',#3387,.T.);
#3765=FACE_BOUND('',#3388,.T.);
#3766=FACE_BOUND('',#3389,.T.);
#3767=FACE_BOUND('',#3390,.T.);
#3768=FACE_BOUND('',#3391,.T.);
#3769=FACE_BOUND('',#3392,.T.);
#3770=FACE_BOUND('',#3393,.T.);
#3771=FACE_BOUND('',#3394,.T.);
#3772=FACE_BOUND('',#3395,.T.);
#3773=FACE_BOUND('',#3396,.T.);
#3774=FACE_BOUND('',#3397,.T.);
#3775=FACE_BOUND('',#3398,.T.);
#3776=FACE_BOUND('',#3399,.T.);
#3777=FACE_BOUND('',#3400,.T.);
#3778=FACE_BOUND('',#3401,.T.);
#3779=FACE_BOUND('',#3402,.T.);
#3780=FACE_BOUND('',#3403,.T.);
#3781=FACE_BOUND('',#3404,.T.);
#3782=FACE_BOUND('',#3405,.T.);
#3783=FACE_BOUND('',#3406,.T.);
#3784=FACE_BOUND('',#3407,.T.);
#3785=FACE_BOUND('',#3408,.T.);
#3786=FACE_BOUND('',#3409,.T.);
#3787=FACE_BOUND('',#3410,.T.);
#3788=FACE_BOUND('',#3411,.T.);
#3789=FACE_BOUND('',#3412,.T.);
#3790=FACE_BOUND('',#3413,.T.);
#3791=FACE_BOUND('',#3414,.T.);
#3792=FACE_BOUND('',#3415,.T.);
#3793=FACE_BOUND('',#3416,.T.);
#3794=FACE_BOUND('',#3417,.T.);
#3795=FACE_BOUND('',#3418,.T.);
#3796=FACE_BOUND('',#3419,.T.);
#3797=FACE_BOUND('',#3420,.T.);
#3798=FACE_BOUND('',#3421,.T.);
#3799=FACE_BOUND('',#3422,.T.);
#3800=FACE_BOUND('',#3423,.T.);
#3801=FACE_BOUND('',#3424,.T.);
#3802=FACE_BOUND('',#3425,.T.);
#3803=FACE_BOUND('',#3426,.T.);
#3804=FACE_BOUND('',#3427,.T.);
#3805=FACE_BOUND('',#3428,.T.);
#3806=FACE_BOUND('',#3429,.T.);
#3807=FACE_BOUND('',#3430,.T.);
#3808=FACE_BOUND('',#3431,.T.);
#3809=FACE_BOUND('',#3432,.T.);
#3810=FACE_BOUND('',#3433,.T.);
#3811=FACE_BOUND('',#3434,.T.);
#3812=FACE_BOUND('',#3435,.T.);
#3813=FACE_BOUND('',#3436,.T.);
#3814=FACE_BOUND('',#3437,.T.);
#3815=FACE_BOUND('',#3438,.T.);
#3816=FACE_BOUND('',#3439,.T.);
#3817=FACE_BOUND('',#3440,.T.);
#3818=FACE_BOUND('',#3441,.T.);
#3819=FACE_BOUND('',#3442,.T.);
#3820=FACE_BOUND('',#3443,.T.);
#3821=FACE_BOUND('',#3444,.T.);
#3822=FACE_BOUND('',#3445,.T.);
#3823=FACE_BOUND('',#3446,.T.);
#3824=FACE_BOUND('',#3447,.T.);
#3825=FACE_BOUND('',#3448,.T.);
#3826=FACE_BOUND('',#3449,.T.);
#3827=FACE_BOUND('',#3450,.T.);
#3828=FACE_BOUND('',#3451,.T.);
#3829=FACE_BOUND('',#3452,.T.);
#3830=FACE_BOUND('',#3453,.T.);
#3831=FACE_BOUND('',#3454,.T.);
#3832=FACE_BOUND('',#3455,.T.);
#3833=FACE_BOUND('',#3456,.T.);
#3834=FACE_BOUND('',#3457,.T.);
#3835=FACE_BOUND('',#3458,.T.);
#3836=FACE_BOUND('',#3459,.T.);
#3837=FACE_BOUND('',#3460,.T.);
#3838=FACE_BOUND('',#3461,.T.);
#3839=FACE_BOUND('',#3462,.T.);
#3840=FACE_BOUND('',#3463,.T.);
#3841=FACE_BOUND('',#3464,.T.);
#3842=FACE_BOUND('',#3465,.T.);
#3843=FACE_BOUND('',#3466,.T.);
#3844=FACE_BOUND('',#3467,.T.);
#3845=FACE_BOUND('',#3468,.T.);
#3846=FACE_BOUND('',#3469,.T.);
#3847=FACE_BOUND('',#3470,.T.);
#3848=FACE_BOUND('',#3471,.T.);
#3849=FACE_BOUND('',#3472,.T.);
#3850=FACE_BOUND('',#3473,.T.);
#3851=FACE_BOUND('',#3474,.T.);
#3852=FACE_BOUND('',#3475,.T.);
#3853=FACE_BOUND('',#3476,.T.);
#3854=FACE_BOUND('',#3477,.T.);
#3855=FACE_BOUND('',#3478,.T.);
#3856=FACE_BOUND('',#3479,.T.);
#3857=FACE_BOUND('',#3480,.T.);
#3858=FACE_BOUND('',#3481,.T.);
#3859=FACE_BOUND('',#3482,.T.);
#3860=FACE_BOUND('',#3483,.T.);
#3861=FACE_BOUND('',#3484,.T.);
#3862=FACE_BOUND('',#3485,.T.);
#3863=FACE_BOUND('',#3486,.T.);
#3864=FACE_BOUND('',#3487,.T.);
#3865=FACE_BOUND('',#3488,.T.);
#3866=FACE_BOUND('',#3489,.T.);
#3867=FACE_BOUND('',#3490,.T.);
#3868=FACE_BOUND('',#3491,.T.);
#3869=FACE_BOUND('',#3492,.T.);
#3870=FACE_BOUND('',#3493,.T.);
#3871=FACE_BOUND('',#3494,.T.);
#3872=FACE_BOUND('',#3495,.T.);
#3873=FACE_BOUND('',#3496,.T.);
#3874=FACE_BOUND('',#3497,.T.);
#3875=FACE_BOUND('',#3498,.T.);
#3876=FACE_BOUND('',#3499,.T.);
#3877=FACE_BOUND('',#3500,.T.);
#3878=FACE_BOUND('',#3501,.T.);
#3879=FACE_BOUND('',#3502,.T.);
#3880=FACE_BOUND('',#3503,.T.);
#3881=FACE_BOUND('',#3504,.T.);
#3882=FACE_BOUND('',#3505,.T.);
#3883=FACE_BOUND('',#3506,.T.);
#3884=FACE_BOUND('',#3507,.T.);
#3885=FACE_BOUND('',#3508,.T.);
#3886=FACE_BOUND('',#3509,.T.);
#3887=FACE_BOUND('',#3510,.T.);
#3888=FACE_BOUND('',#3511,.T.);
#3889=FACE_BOUND('',#3512,.T.);
#3890=FACE_BOUND('',#3513,.T.);
#3891=FACE_BOUND('',#3514,.T.);
#3892=FACE_BOUND('',#3515,.T.);
#3893=FACE_BOUND('',#3516,.T.);
#3894=FACE_BOUND('',#3517,.T.);
#3895=FACE_BOUND('',#3518,.T.);
#3896=FACE_BOUND('',#3519,.T.);
#3897=FACE_BOUND('',#3520,.T.);
#3898=FACE_BOUND('',#3521,.T.);
#3899=FACE_BOUND('',#3522,.T.);
#3900=FACE_BOUND('',#3523,.T.);
#3901=FACE_BOUND('',#3524,.T.);
#3902=FACE_BOUND('',#3525,.T.);
#3903=FACE_BOUND('',#3526,.T.);
#3904=FACE_BOUND('',#3527,.T.);
#3905=FACE_BOUND('',#3528,.T.);
#3906=FACE_BOUND('',#3529,.T.);
#3907=FACE_BOUND('',#3530,.T.);
#3908=FACE_BOUND('',#3531,.T.);
#3909=FACE_BOUND('',#3532,.T.);
#3910=FACE_BOUND('',#3533,.T.);
#3911=FACE_BOUND('',#3534,.T.);
#3912=FACE_BOUND('',#3535,.T.);
#3913=FACE_BOUND('',#3536,.T.);
#3914=FACE_BOUND('',#3537,.T.);
#3915=FACE_BOUND('',#3538,.T.);
#3916=FACE_BOUND('',#3539,.T.);
#3917=FACE_BOUND('',#3540,.T.);
#3918=FACE_BOUND('',#3541,.T.);
#3919=FACE_BOUND('',#3542,.T.);
#3920=FACE_BOUND('',#3543,.T.);
#3921=FACE_BOUND('',#3544,.T.);
#3922=FACE_BOUND('',#3545,.T.);
#3923=FACE_BOUND('',#3546,.T.);
#3924=FACE_BOUND('',#3547,.T.);
#3925=FACE_BOUND('',#3548,.T.);
#3926=FACE_BOUND('',#3549,.T.);
#3927=FACE_BOUND('',#3550,.T.);
#3928=FACE_BOUND('',#3551,.T.);
#3929=FACE_BOUND('',#3552,.T.);
#3930=FACE_BOUND('',#3553,.T.);
#3931=FACE_BOUND('',#3554,.T.);
#3932=FACE_BOUND('',#3555,.T.);
#3933=FACE_BOUND('',#3556,.T.);
#3934=FACE_BOUND('',#3557,.T.);
#3935=FACE_BOUND('',#3558,.T.);
#3936=FACE_BOUND('',#3559,.T.);
#3937=FACE_BOUND('',#3560,.T.);
#3938=FACE_BOUND('',#3561,.T.);
#3939=FACE_BOUND('',#3562,.T.);
#3940=FACE_BOUND('',#3563,.T.);
#3941=FACE_BOUND('',#3564,.T.);
#3942=FACE_BOUND('',#3565,.T.);
#3943=FACE_BOUND('',#3566,.T.);
#3944=PLANE('',#4485);
#3945=PLANE('',#4486);
#3946=PLANE('',#4487);
#3947=PLANE('',#4488);
#3948=PLANE('',#4489);
#3949=PLANE('',#4490);
#3950=PLANE('',#4491);
#3951=PLANE('',#4496);
#3952=PLANE('',#4510);
#3953=PLANE('',#4514);
#3954=PLANE('',#4517);
#3955=PLANE('',#4526);
#3956=PLANE('',#4530);
#3957=PLANE('',#4531);
#3958=PLANE('',#4532);
#3959=PLANE('',#4542);
#3960=PLANE('',#4546);
#3961=PLANE('',#4550);
#3962=PLANE('',#4554);
#3963=PLANE('',#4558);
#3964=PLANE('',#4562);
#3965=PLANE('',#4566);
#3966=PLANE('',#4570);
#3967=PLANE('',#4574);
#3968=PLANE('',#4575);
#3969=PLANE('',#4576);
#3970=PLANE('',#4579);
#3971=PLANE('',#4582);
#3972=PLANE('',#4588);
#3973=PLANE('',#4591);
#3974=PLANE('',#4616);
#3975=PLANE('',#4617);
#3976=PLANE('',#4627);
#3977=PLANE('',#4636);
#3978=PLANE('',#4637);
#3979=PLANE('',#4638);
#3980=PLANE('',#4639);
#3981=PLANE('',#4643);
#3982=PLANE('',#4647);
#3983=PLANE('',#4648);
#3984=PLANE('',#4651);
#3985=PLANE('',#4656);
#3986=PLANE('',#4661);
#3987=PLANE('',#4662);
#3988=PLANE('',#4673);
#3989=PLANE('',#4677);
#3990=PLANE('',#4692);
#3991=PLANE('',#4699);
#3992=PLANE('',#4706);
#3993=PLANE('',#4723);
#3994=PLANE('',#4730);
#3995=PLANE('',#4737);
#3996=PLANE('',#4757);
#3997=PLANE('',#4758);
#3998=PLANE('',#4762);
#3999=PLANE('',#4767);
#4000=PLANE('',#4772);
#4001=PLANE('',#4775);
#4002=PLANE('',#4780);
#4003=PLANE('',#4785);
#4004=PLANE('',#4806);
#4005=PLANE('',#4809);
#4006=PLANE('',#4938);
#4007=PLANE('',#4939);
#4008=PLANE('',#4941);
#4009=PLANE('',#4948);
#4010=PLANE('',#4949);
#4011=PLANE('',#4950);
#4012=PLANE('',#4958);
#4013=PLANE('',#4959);
#4014=PLANE('',#4964);
#4015=PLANE('',#4971);
#4016=PLANE('',#4973);
#4017=PLANE('',#4976);
#4018=PLANE('',#4978);
#4019=PLANE('',#4983);
#4020=PLANE('',#5016);
#4021=PLANE('',#5017);
#4022=PLANE('',#5019);
#4023=PLANE('',#5026);
#4024=PLANE('',#5029);
#4025=PLANE('',#5031);
#4026=PLANE('',#5035);
#4027=PLANE('',#5042);
#4028=PLANE('',#5047);
#4029=PLANE('',#5048);
#4030=PLANE('',#5049);
#4031=PLANE('',#5050);
#4032=PLANE('',#5052);
#4033=PLANE('',#5059);
#4034=PLANE('',#5060);
#4035=PLANE('',#5061);
#4036=ADVANCED_FACE('',(#3567),#3944,.T.);
#4037=ADVANCED_FACE('',(#3568),#3945,.T.);
#4038=ADVANCED_FACE('',(#3569),#3946,.T.);
#4039=ADVANCED_FACE('',(#3570),#3947,.T.);
#4040=ADVANCED_FACE('',(#3571),#3948,.T.);
#4041=ADVANCED_FACE('',(#3572),#3949,.T.);
#4042=ADVANCED_FACE('',(#3573,#3574),#3950,.F.);
#4043=ADVANCED_FACE('',(#3575,#3576),#204,.T.);
#4044=ADVANCED_FACE('',(#3577),#3951,.T.);
#4045=ADVANCED_FACE('',(#3578),#193,.T.);
#4046=ADVANCED_FACE('',(#3579),#194,.T.);
#4047=ADVANCED_FACE('',(#3580),#195,.T.);
#4048=ADVANCED_FACE('',(#3581),#196,.T.);
#4049=ADVANCED_FACE('',(#3582),#197,.T.);
#4050=ADVANCED_FACE('',(#3583),#198,.T.);
#4051=ADVANCED_FACE('',(#3584),#3952,.T.);
#4052=ADVANCED_FACE('',(#3585,#3586),#139,.F.);
#4053=ADVANCED_FACE('',(#3587,#3588),#199,.T.);
#4054=ADVANCED_FACE('',(#3589,#3590),#3953,.T.);
#4055=ADVANCED_FACE('',(#3591,#3592),#3954,.F.);
#4056=ADVANCED_FACE('',(#3593,#3594),#205,.T.);
#4057=ADVANCED_FACE('',(#3595,#3596),#206,.F.);
#4058=ADVANCED_FACE('',(#3597),#207,.T.);
#4059=ADVANCED_FACE('',(#3598),#3955,.F.);
#4060=ADVANCED_FACE('',(#3599),#208,.F.);
#4061=ADVANCED_FACE('',(#3600),#3956,.F.);
#4062=ADVANCED_FACE('',(#3601),#3957,.T.);
#4063=ADVANCED_FACE('',(#3602),#3958,.F.);
#4064=ADVANCED_FACE('',(#3603,#3604),#209,.F.);
#4065=ADVANCED_FACE('',(#3605,#3606,#3607,#3608),#210,.T.);
#4066=ADVANCED_FACE('',(#3609,#3610,#3611,#3612),#211,.F.);
#4067=ADVANCED_FACE('',(#3613),#3959,.T.);
#4068=ADVANCED_FACE('',(#3614,#3615),#212,.T.);
#4069=ADVANCED_FACE('',(#3616,#3617),#3960,.T.);
#4070=ADVANCED_FACE('',(#3618,#3619),#213,.T.);
#4071=ADVANCED_FACE('',(#3620,#3621),#3961,.T.);
#4072=ADVANCED_FACE('',(#3622,#3623),#214,.T.);
#4073=ADVANCED_FACE('',(#3624,#3625),#3962,.T.);
#4074=ADVANCED_FACE('',(#3626,#3627),#215,.T.);
#4075=ADVANCED_FACE('',(#3628,#3629),#3963,.T.);
#4076=ADVANCED_FACE('',(#3630,#3631),#216,.T.);
#4077=ADVANCED_FACE('',(#3632,#3633),#3964,.T.);
#4078=ADVANCED_FACE('',(#3634,#3635),#217,.T.);
#4079=ADVANCED_FACE('',(#3636,#3637),#3965,.T.);
#4080=ADVANCED_FACE('',(#3638,#3639),#218,.T.);
#4081=ADVANCED_FACE('',(#3640,#3641),#3966,.T.);
#4082=ADVANCED_FACE('',(#3642,#3643),#219,.T.);
#4083=ADVANCED_FACE('',(#3644,#3645),#3967,.T.);
#4084=ADVANCED_FACE('',(#3646,#3647),#3968,.T.);
#4085=ADVANCED_FACE('',(#3648),#3969,.T.);
#4086=ADVANCED_FACE('',(#3649,#3650),#220,.F.);
#4087=ADVANCED_FACE('',(#3651,#3652),#3970,.F.);
#4088=ADVANCED_FACE('',(#3653,#3654),#221,.F.);
#4089=ADVANCED_FACE('',(#3655,#3656),#3971,.F.);
#4090=ADVANCED_FACE('',(#3657,#3658),#222,.F.);
#4091=ADVANCED_FACE('',(#3659,#3660),#3972,.T.);
#4092=ADVANCED_FACE('',(#3661,#3662),#3973,.F.);
#4093=ADVANCED_FACE('',(#3663,#3664),#223,.F.);
#4094=ADVANCED_FACE('',(#3665,#3666),#224,.T.);
#4095=ADVANCED_FACE('',(#3667),#225,.T.);
#4096=ADVANCED_FACE('',(#3668),#140,.T.);
#4097=ADVANCED_FACE('',(#3669),#141,.T.);
#4098=ADVANCED_FACE('',(#3670),#226,.T.);
#4099=ADVANCED_FACE('',(#3671),#227,.T.);
#4100=ADVANCED_FACE('',(#3672),#228,.T.);
#4101=ADVANCED_FACE('',(#3673),#229,.T.);
#4102=ADVANCED_FACE('',(#3674),#230,.T.);
#4103=ADVANCED_FACE('',(#3675),#231,.T.);
#4104=ADVANCED_FACE('',(#3676),#3974,.T.);
#4105=ADVANCED_FACE('',(#3677),#3975,.T.);
#4106=ADVANCED_FACE('',(#3678),#142,.F.);
#4107=ADVANCED_FACE('',(#3679),#232,.T.);
#4108=ADVANCED_FACE('',(#3680),#143,.F.);
#4109=ADVANCED_FACE('',(#3681),#3976,.T.);
#4110=ADVANCED_FACE('',(#3682),#233,.T.);
#4111=ADVANCED_FACE('',(#3683),#234,.F.);
#4112=ADVANCED_FACE('',(#3684),#235,.T.);
#4113=ADVANCED_FACE('',(#3685),#236,.T.);
#4114=ADVANCED_FACE('',(#3686),#3977,.F.);
#4115=ADVANCED_FACE('',(#3687),#3978,.F.);
#4116=ADVANCED_FACE('',(#3688),#3979,.T.);
#4117=ADVANCED_FACE('',(#3689,#3690),#3980,.F.);
#4118=ADVANCED_FACE('',(#3691,#3692),#237,.F.);
#4119=ADVANCED_FACE('',(#3693,#3694),#3981,.F.);
#4120=ADVANCED_FACE('',(#3695,#3696),#238,.F.);
#4121=ADVANCED_FACE('',(#3697,#3698),#3982,.F.);
#4122=ADVANCED_FACE('',(#3699,#3700),#3983,.F.);
#4123=ADVANCED_FACE('',(#3701),#3984,.T.);
#4124=ADVANCED_FACE('',(#3702),#3985,.F.);
#4125=ADVANCED_FACE('',(#3703),#3986,.F.);
#4126=ADVANCED_FACE('',(#3704),#3987,.T.);
#4127=ADVANCED_FACE('',(#3705),#239,.F.);
#4128=ADVANCED_FACE('',(#3706,#3707),#240,.F.);
#4129=ADVANCED_FACE('',(#3708,#3709),#241,.F.);
#4130=ADVANCED_FACE('',(#3710),#242,.T.);
#4131=ADVANCED_FACE('',(#3711),#3988,.T.);
#4132=ADVANCED_FACE('',(#3712),#243,.T.);
#4133=ADVANCED_FACE('',(#3713),#3989,.T.);
#4134=ADVANCED_FACE('',(#3714),#244,.T.);
#4135=ADVANCED_FACE('',(#3715),#245,.T.);
#4136=ADVANCED_FACE('',(#3716),#246,.T.);
#4137=ADVANCED_FACE('',(#3717),#247,.T.);
#4138=ADVANCED_FACE('',(#3718),#144,.F.);
#4139=ADVANCED_FACE('',(#3719),#145,.F.);
#4140=ADVANCED_FACE('',(#3720),#3990,.F.);
#4141=ADVANCED_FACE('',(#3721),#3991,.T.);
#4142=ADVANCED_FACE('',(#3722,#3723),#3992,.T.);
#4143=ADVANCED_FACE('',(#3724),#248,.F.);
#4144=ADVANCED_FACE('',(#3725),#249,.F.);
#4145=ADVANCED_FACE('',(#3726,#3727),#3993,.F.);
#4146=ADVANCED_FACE('',(#3728),#3994,.F.);
#4147=ADVANCED_FACE('',(#3729),#3995,.T.);
#4148=ADVANCED_FACE('',(#3730,#3731),#250,.F.);
#4149=ADVANCED_FACE('',(#3732),#251,.T.);
#4150=ADVANCED_FACE('',(#3733,#3734),#252,.F.);
#4151=ADVANCED_FACE('',(#3735),#3996,.F.);
#4152=ADVANCED_FACE('',(#3736),#3997,.T.);
#4153=ADVANCED_FACE('',(#3737,#3738),#253,.F.);
#4154=ADVANCED_FACE('',(#3739),#3998,.F.);
#4155=ADVANCED_FACE('',(#3740),#254,.F.);
#4156=ADVANCED_FACE('',(#3741),#3999,.T.);
#4157=ADVANCED_FACE('',(#3742),#255,.F.);
#4158=ADVANCED_FACE('',(#3743),#4000,.T.);
#4159=ADVANCED_FACE('',(#3744),#4001,.T.);
#4160=ADVANCED_FACE('',(#3745),#256,.F.);
#4161=ADVANCED_FACE('',(#3746),#4002,.F.);
#4162=ADVANCED_FACE('',(#3747),#257,.F.);
#4163=ADVANCED_FACE('',(#3748),#4003,.T.);
#4164=ADVANCED_FACE('',(#3749),#146,.F.);
#4165=ADVANCED_FACE('',(#3750),#258,.F.);
#4166=ADVANCED_FACE('',(#3751),#147,.F.);
#4167=ADVANCED_FACE('',(#3752),#148,.F.);
#4168=ADVANCED_FACE('',(#3753),#259,.F.);
#4169=ADVANCED_FACE('',(#3754),#149,.F.);
#4170=ADVANCED_FACE('',(#3755),#150,.F.);
#4171=ADVANCED_FACE('',(#3756),#151,.F.);
#4172=ADVANCED_FACE('',(#3757),#152,.F.);
#4173=ADVANCED_FACE('',(#3758),#260,.F.);
#4174=ADVANCED_FACE('',(#3759),#261,.F.);
#4175=ADVANCED_FACE('',(#3760),#153,.F.);
#4176=ADVANCED_FACE('',(#3761,#3762),#4004,.T.);
#4177=ADVANCED_FACE('',(#3763,#3764),#4005,.T.);
#4178=ADVANCED_FACE('',(#3765),#154,.T.);
#4179=ADVANCED_FACE('',(#3766),#262,.T.);
#4180=ADVANCED_FACE('',(#3767),#27,.T.);
#4181=ADVANCED_FACE('',(#3768),#155,.T.);
#4182=ADVANCED_FACE('',(#3769),#156,.T.);
#4183=ADVANCED_FACE('',(#3770),#28,.T.);
#4184=ADVANCED_FACE('',(#3771),#263,.T.);
#4185=ADVANCED_FACE('',(#3772),#264,.T.);
#4186=ADVANCED_FACE('',(#3773),#157,.T.);
#4187=ADVANCED_FACE('',(#3774),#29,.T.);
#4188=ADVANCED_FACE('',(#3775),#158,.T.);
#4189=ADVANCED_FACE('',(#3776),#30,.T.);
#4190=ADVANCED_FACE('',(#3777),#159,.T.);
#4191=ADVANCED_FACE('',(#3778),#265,.T.);
#4192=ADVANCED_FACE('',(#3779),#160,.T.);
#4193=ADVANCED_FACE('',(#3780),#31,.T.);
#4194=ADVANCED_FACE('',(#3781),#161,.T.);
#4195=ADVANCED_FACE('',(#3782),#32,.T.);
#4196=ADVANCED_FACE('',(#3783),#162,.T.);
#4197=ADVANCED_FACE('',(#3784),#266,.T.);
#4198=ADVANCED_FACE('',(#3785),#163,.T.);
#4199=ADVANCED_FACE('',(#3786),#33,.T.);
#4200=ADVANCED_FACE('',(#3787),#164,.T.);
#4201=ADVANCED_FACE('',(#3788),#267,.T.);
#4202=ADVANCED_FACE('',(#3789),#34,.T.);
#4203=ADVANCED_FACE('',(#3790),#165,.T.);
#4204=ADVANCED_FACE('',(#3791),#166,.T.);
#4205=ADVANCED_FACE('',(#3792),#35,.T.);
#4206=ADVANCED_FACE('',(#3793),#268,.T.);
#4207=ADVANCED_FACE('',(#3794),#167,.F.);
#4208=ADVANCED_FACE('',(#3795),#168,.T.);
#4209=ADVANCED_FACE('',(#3796),#36,.T.);
#4210=ADVANCED_FACE('',(#3797),#169,.T.);
#4211=ADVANCED_FACE('',(#3798),#37,.T.);
#4212=ADVANCED_FACE('',(#3799),#170,.T.);
#4213=ADVANCED_FACE('',(#3800),#269,.T.);
#4214=ADVANCED_FACE('',(#3801),#171,.T.);
#4215=ADVANCED_FACE('',(#3802),#38,.T.);
#4216=ADVANCED_FACE('',(#3803),#172,.T.);
#4217=ADVANCED_FACE('',(#3804),#39,.T.);
#4218=ADVANCED_FACE('',(#3805),#173,.T.);
#4219=ADVANCED_FACE('',(#3806),#270,.T.);
#4220=ADVANCED_FACE('',(#3807),#174,.T.);
#4221=ADVANCED_FACE('',(#3808),#40,.T.);
#4222=ADVANCED_FACE('',(#3809),#175,.F.);
#4223=ADVANCED_FACE('',(#3810),#271,.F.);
#4224=ADVANCED_FACE('',(#3811),#272,.F.);
#4225=ADVANCED_FACE('',(#3812),#176,.F.);
#4226=ADVANCED_FACE('',(#3813),#15,.T.);
#4227=ADVANCED_FACE('',(#3814),#177,.T.);
#4228=ADVANCED_FACE('',(#3815),#16,.T.);
#4229=ADVANCED_FACE('',(#3816),#17,.T.);
#4230=ADVANCED_FACE('',(#3817),#273,.T.);
#4231=ADVANCED_FACE('',(#3818),#18,.T.);
#4232=ADVANCED_FACE('',(#3819),#19,.T.);
#4233=ADVANCED_FACE('',(#3820),#274,.T.);
#4234=ADVANCED_FACE('',(#3821),#20,.T.);
#4235=ADVANCED_FACE('',(#3822),#21,.T.);
#4236=ADVANCED_FACE('',(#3823),#178,.T.);
#4237=ADVANCED_FACE('',(#3824),#22,.T.);
#4238=ADVANCED_FACE('',(#3825),#179,.T.);
#4239=ADVANCED_FACE('',(#3826),#180,.T.);
#4240=ADVANCED_FACE('',(#3827),#181,.T.);
#4241=ADVANCED_FACE('',(#3828),#23,.T.);
#4242=ADVANCED_FACE('',(#3829),#24,.T.);
#4243=ADVANCED_FACE('',(#3830),#182,.T.);
#4244=ADVANCED_FACE('',(#3831),#183,.T.);
#4245=ADVANCED_FACE('',(#3832),#275,.T.);
#4246=ADVANCED_FACE('',(#3833,#3834),#184,.F.);
#4247=ADVANCED_FACE('',(#3835,#3836),#185,.T.);
#4248=ADVANCED_FACE('',(#3837,#3838),#186,.T.);
#4249=ADVANCED_FACE('',(#3839),#187,.T.);
#4250=ADVANCED_FACE('',(#3840),#188,.T.);
#4251=ADVANCED_FACE('',(#3841),#189,.T.);
#4252=ADVANCED_FACE('',(#3842),#25,.T.);
#4253=ADVANCED_FACE('',(#3843),#26,.T.);
#4254=ADVANCED_FACE('',(#3844),#190,.T.);
#4255=ADVANCED_FACE('',(#3845),#191,.T.);
#4256=ADVANCED_FACE('',(#3846),#276,.T.);
#4257=ADVANCED_FACE('',(#3847,#3848),#192,.F.);
#4258=ADVANCED_FACE('',(#3849,#3850),#4006,.T.);
#4259=ADVANCED_FACE('',(#3851,#3852),#4007,.T.);
#4260=ADVANCED_FACE('',(#3853),#4008,.T.);
#4261=ADVANCED_FACE('',(#3854),#277,.F.);
#4262=ADVANCED_FACE('',(#3855),#278,.T.);
#4263=ADVANCED_FACE('',(#3856),#4009,.T.);
#4264=ADVANCED_FACE('',(#3857),#4010,.T.);
#4265=ADVANCED_FACE('',(#3858),#4011,.T.);
#4266=ADVANCED_FACE('',(#3859,#3860),#279,.F.);
#4267=ADVANCED_FACE('',(#3861,#3862),#280,.T.);
#4268=ADVANCED_FACE('',(#3863,#3864),#4012,.T.);
#4269=ADVANCED_FACE('',(#3865,#3866),#4013,.F.);
#4270=ADVANCED_FACE('',(#3867,#3868),#281,.T.);
#4271=ADVANCED_FACE('',(#3869,#3870),#4014,.T.);
#4272=ADVANCED_FACE('',(#3871,#3872),#282,.T.);
#4273=ADVANCED_FACE('',(#3873),#4015,.F.);
#4274=ADVANCED_FACE('',(#3874),#4016,.T.);
#4275=ADVANCED_FACE('',(#3875),#283,.T.);
#4276=ADVANCED_FACE('',(#3876),#4017,.T.);
#4277=ADVANCED_FACE('',(#3877),#4018,.F.);
#4278=ADVANCED_FACE('',(#3878,#3879,#3880),#284,.T.);
#4279=ADVANCED_FACE('',(#3881),#285,.F.);
#4280=ADVANCED_FACE('',(#3882),#4019,.F.);
#4281=ADVANCED_FACE('',(#3883),#286,.T.);
#4282=ADVANCED_FACE('',(#3884),#200,.T.);
#4283=ADVANCED_FACE('',(#3885),#201,.T.);
#4284=ADVANCED_FACE('',(#3886),#287,.T.);
#4285=ADVANCED_FACE('',(#3887,#3888),#288,.F.);
#4286=ADVANCED_FACE('',(#3889,#3890),#289,.F.);
#4287=ADVANCED_FACE('',(#3891),#290,.T.);
#4288=ADVANCED_FACE('',(#3892,#3893),#291,.T.);
#4289=ADVANCED_FACE('',(#3894,#3895,#3896,#3897),#292,.T.);
#4290=ADVANCED_FACE('',(#3898,#3899),#293,.F.);
#4291=ADVANCED_FACE('',(#3900,#3901,#3902,#3903),#294,.T.);
#4292=ADVANCED_FACE('',(#3904,#3905),#295,.F.);
#4293=ADVANCED_FACE('',(#3906,#3907),#4020,.F.);
#4294=ADVANCED_FACE('',(#3908),#4021,.F.);
#4295=ADVANCED_FACE('',(#3909,#3910),#4022,.T.);
#4296=ADVANCED_FACE('',(#3911),#296,.F.);
#4297=ADVANCED_FACE('',(#3912),#297,.F.);
#4298=ADVANCED_FACE('',(#3913,#3914),#298,.F.);
#4299=ADVANCED_FACE('',(#3915),#299,.F.);
#4300=ADVANCED_FACE('',(#3916),#4023,.T.);
#4301=ADVANCED_FACE('',(#3917),#300,.T.);
#4302=ADVANCED_FACE('',(#3918),#4024,.T.);
#4303=ADVANCED_FACE('',(#3919),#4025,.F.);
#4304=ADVANCED_FACE('',(#3920,#3921),#301,.T.);
#4305=ADVANCED_FACE('',(#3922),#302,.F.);
#4306=ADVANCED_FACE('',(#3923),#4026,.F.);
#4307=ADVANCED_FACE('',(#3924),#303,.T.);
#4308=ADVANCED_FACE('',(#3925),#202,.T.);
#4309=ADVANCED_FACE('',(#3926,#3927),#4027,.T.);
#4310=ADVANCED_FACE('',(#3928),#203,.T.);
#4311=ADVANCED_FACE('',(#3929),#304,.T.);
#4312=ADVANCED_FACE('',(#3930),#305,.T.);
#4313=ADVANCED_FACE('',(#3931,#3932),#4028,.F.);
#4314=ADVANCED_FACE('',(#3933),#4029,.F.);
#4315=ADVANCED_FACE('',(#3934,#3935),#4030,.T.);
#4316=ADVANCED_FACE('',(#3936,#3937),#4031,.F.);
#4317=ADVANCED_FACE('',(#3938),#4032,.T.);
#4318=ADVANCED_FACE('',(#3939),#306,.F.);
#4319=ADVANCED_FACE('',(#3940),#307,.T.);
#4320=ADVANCED_FACE('',(#3941),#4033,.T.);
#4321=ADVANCED_FACE('',(#3942),#4034,.F.);
#4322=ADVANCED_FACE('',(#3943),#4035,.F.);
#4323=CLOSED_SHELL('',(#4036,#4037,#4038,#4039,#4040,#4041,#4042,#4043,
#4044,#4045,#4046,#4047,#4048,#4049,#4050,#4051,#4052,#4053));
#4324=CLOSED_SHELL('',(#4054,#4055,#4056,#4057));
#4325=CLOSED_SHELL('',(#4058,#4059,#4060,#4061,#4062,#4063));
#4326=CLOSED_SHELL('',(#4064,#4065,#4066,#4067,#4068,#4069,#4070,#4071,
#4072,#4073,#4074,#4075,#4076,#4077,#4078,#4079,#4080,#4081,#4082,#4083,
#4084,#4085,#4086,#4087,#4088,#4089,#4090));
#4327=CLOSED_SHELL('',(#4091,#4092,#4093,#4094));
#4328=CLOSED_SHELL('',(#4095,#4096,#4097,#4098,#4099,#4100,#4101,#4102,
#4103,#4104,#4105,#4106,#4107,#4108,#4109,#4110,#4111,#4112,#4113,#4114,
#4115,#4116,#4117,#4118,#4119,#4120,#4121,#4122));
#4329=CLOSED_SHELL('',(#4123,#4124,#4125,#4126,#4127,#4128,#4129,#4130,
#4131,#4132,#4133,#4134,#4135,#4136,#4137,#4138,#4139,#4140,#4141,#4142,
#4143,#4144,#4145,#4146,#4147,#4148,#4149,#4150,#4151,#4152,#4153,#4154,
#4155,#4156,#4157,#4158,#4159,#4160,#4161,#4162,#4163,#4164,#4165,#4166,
#4167,#4168,#4169,#4170,#4171,#4172,#4173,#4174,#4175,#4176,#4177,#4178,
#4179,#4180,#4181,#4182,#4183,#4184,#4185,#4186,#4187,#4188,#4189,#4190,
#4191,#4192,#4193,#4194,#4195,#4196,#4197,#4198,#4199,#4200,#4201,#4202,
#4203,#4204,#4205,#4206,#4207,#4208,#4209,#4210,#4211,#4212,#4213,#4214,
#4215,#4216,#4217,#4218,#4219,#4220,#4221,#4222,#4223,#4224,#4225,#4226,
#4227,#4228,#4229,#4230,#4231,#4232,#4233,#4234,#4235,#4236,#4237,#4238,
#4239,#4240,#4241,#4242,#4243,#4244,#4245,#4246,#4247,#4248,#4249,#4250,
#4251,#4252,#4253,#4254,#4255,#4256,#4257,#4258,#4259));
#4330=CLOSED_SHELL('',(#4260,#4261,#4262,#4263,#4264,#4265));
#4331=CLOSED_SHELL('',(#4266,#4267,#4268,#4269));
#4332=CLOSED_SHELL('',(#4270,#4271,#4272,#4273,#4274,#4275,#4276,#4277,
#4278,#4279,#4280,#4281,#4282,#4283,#4284,#4285,#4286,#4287,#4288,#4289,
#4290,#4291,#4292,#4293,#4294,#4295,#4296,#4297,#4298,#4299,#4300,#4301,
#4302,#4303,#4304,#4305,#4306,#4307,#4308,#4309,#4310,#4311,#4312,#4313,
#4314,#4315,#4316));
#4333=CLOSED_SHELL('',(#4317,#4318,#4319,#4320,#4321,#4322));
#4334=STYLED_ITEM('',(#4345),#4449);
#4335=STYLED_ITEM('',(#4346),#4450);
#4336=STYLED_ITEM('',(#4347),#4451);
#4337=STYLED_ITEM('',(#4348),#4452);
#4338=STYLED_ITEM('',(#4349),#4453);
#4339=STYLED_ITEM('',(#4350),#4454);
#4340=STYLED_ITEM('',(#4351),#4455);
#4341=STYLED_ITEM('',(#4352),#4456);
#4342=STYLED_ITEM('',(#4353),#4457);
#4343=STYLED_ITEM('',(#4354),#4458);
#4344=STYLED_ITEM('',(#4360),#4459);
#4345=PRESENTATION_STYLE_ASSIGNMENT((#4361));
#4346=PRESENTATION_STYLE_ASSIGNMENT((#4362));
#4347=PRESENTATION_STYLE_ASSIGNMENT((#4363));
#4348=PRESENTATION_STYLE_ASSIGNMENT((#4364));
#4349=PRESENTATION_STYLE_ASSIGNMENT((#4365));
#4350=PRESENTATION_STYLE_ASSIGNMENT((#4366));
#4351=PRESENTATION_STYLE_ASSIGNMENT((#4367));
#4352=PRESENTATION_STYLE_ASSIGNMENT((#4368));
#4353=PRESENTATION_STYLE_ASSIGNMENT((#4369));
#4354=PRESENTATION_STYLE_ASSIGNMENT((#4370));
#4355=PRESENTATION_STYLE_ASSIGNMENT((#4371));
#4356=PRESENTATION_STYLE_ASSIGNMENT((#4372));
#4357=PRESENTATION_STYLE_ASSIGNMENT((#4373));
#4358=PRESENTATION_STYLE_ASSIGNMENT((#4374));
#4359=PRESENTATION_STYLE_ASSIGNMENT((#4375));
#4360=PRESENTATION_STYLE_ASSIGNMENT((#4376));
#4361=SURFACE_STYLE_USAGE(.BOTH.,#4377);
#4362=SURFACE_STYLE_USAGE(.BOTH.,#4378);
#4363=SURFACE_STYLE_USAGE(.BOTH.,#4379);
#4364=SURFACE_STYLE_USAGE(.BOTH.,#4380);
#4365=SURFACE_STYLE_USAGE(.BOTH.,#4381);
#4366=SURFACE_STYLE_USAGE(.BOTH.,#4382);
#4367=SURFACE_STYLE_USAGE(.BOTH.,#4383);
#4368=SURFACE_STYLE_USAGE(.BOTH.,#4384);
#4369=SURFACE_STYLE_USAGE(.BOTH.,#4385);
#4370=SURFACE_STYLE_USAGE(.BOTH.,#4386);
#4371=SURFACE_STYLE_USAGE(.BOTH.,#4387);
#4372=SURFACE_STYLE_USAGE(.BOTH.,#4388);
#4373=SURFACE_STYLE_USAGE(.BOTH.,#4389);
#4374=SURFACE_STYLE_USAGE(.BOTH.,#4390);
#4375=SURFACE_STYLE_USAGE(.BOTH.,#4391);
#4376=SURFACE_STYLE_USAGE(.BOTH.,#4392);
#4377=SURFACE_SIDE_STYLE('',(#4393));
#4378=SURFACE_SIDE_STYLE('',(#4394));
#4379=SURFACE_SIDE_STYLE('',(#4395));
#4380=SURFACE_SIDE_STYLE('',(#4396));
#4381=SURFACE_SIDE_STYLE('',(#4397));
#4382=SURFACE_SIDE_STYLE('',(#4398));
#4383=SURFACE_SIDE_STYLE('',(#4399));
#4384=SURFACE_SIDE_STYLE('',(#4400));
#4385=SURFACE_SIDE_STYLE('',(#4401));
#4386=SURFACE_SIDE_STYLE('',(#4402));
#4387=SURFACE_SIDE_STYLE('',(#4403));
#4388=SURFACE_SIDE_STYLE('',(#4404));
#4389=SURFACE_SIDE_STYLE('',(#4405));
#4390=SURFACE_SIDE_STYLE('',(#4406));
#4391=SURFACE_SIDE_STYLE('',(#4407));
#4392=SURFACE_SIDE_STYLE('',(#4408));
#4393=SURFACE_STYLE_FILL_AREA(#4409);
#4394=SURFACE_STYLE_FILL_AREA(#4410);
#4395=SURFACE_STYLE_FILL_AREA(#4411);
#4396=SURFACE_STYLE_FILL_AREA(#4412);
#4397=SURFACE_STYLE_FILL_AREA(#4413);
#4398=SURFACE_STYLE_FILL_AREA(#4414);
#4399=SURFACE_STYLE_FILL_AREA(#4415);
#4400=SURFACE_STYLE_FILL_AREA(#4416);
#4401=SURFACE_STYLE_FILL_AREA(#4417);
#4402=SURFACE_STYLE_FILL_AREA(#4418);
#4403=SURFACE_STYLE_FILL_AREA(#4419);
#4404=SURFACE_STYLE_FILL_AREA(#4420);
#4405=SURFACE_STYLE_FILL_AREA(#4421);
#4406=SURFACE_STYLE_FILL_AREA(#4422);
#4407=SURFACE_STYLE_FILL_AREA(#4423);
#4408=SURFACE_STYLE_FILL_AREA(#4424);
#4409=FILL_AREA_STYLE('',(#4425));
#4410=FILL_AREA_STYLE('',(#4426));
#4411=FILL_AREA_STYLE('',(#4427));
#4412=FILL_AREA_STYLE('',(#4428));
#4413=FILL_AREA_STYLE('',(#4429));
#4414=FILL_AREA_STYLE('',(#4430));
#4415=FILL_AREA_STYLE('',(#4431));
#4416=FILL_AREA_STYLE('',(#4432));
#4417=FILL_AREA_STYLE('',(#4433));
#4418=FILL_AREA_STYLE('',(#4434));
#4419=FILL_AREA_STYLE('',(#4435));
#4420=FILL_AREA_STYLE('',(#4436));
#4421=FILL_AREA_STYLE('',(#4437));
#4422=FILL_AREA_STYLE('',(#4438));
#4423=FILL_AREA_STYLE('',(#4439));
#4424=FILL_AREA_STYLE('',(#4440));
#4425=FILL_AREA_STYLE_COLOUR('',#4441);
#4426=FILL_AREA_STYLE_COLOUR('',#4442);
#4427=FILL_AREA_STYLE_COLOUR('',#4443);
#4428=FILL_AREA_STYLE_COLOUR('',#4444);
#4429=FILL_AREA_STYLE_COLOUR('',#4442);
#4430=FILL_AREA_STYLE_COLOUR('',#4442);
#4431=FILL_AREA_STYLE_COLOUR('',#4442);
#4432=FILL_AREA_STYLE_COLOUR('',#4445);
#4433=FILL_AREA_STYLE_COLOUR('',#4446);
#4434=FILL_AREA_STYLE_COLOUR('',#4447);
#4435=FILL_AREA_STYLE_COLOUR('',#4448);
#4436=FILL_AREA_STYLE_COLOUR('',#4448);
#4437=FILL_AREA_STYLE_COLOUR('',#4448);
#4438=FILL_AREA_STYLE_COLOUR('',#4448);
#4439=FILL_AREA_STYLE_COLOUR('',#4448);
#4440=FILL_AREA_STYLE_COLOUR('',#4445);
#4441=COLOUR_RGB('', 0.66274510, 0.83137255, 0.94901961);
#4442=COLOUR_RGB('', 0.31764706, 0.68627451, 0.89019608);
#4443=COLOUR_RGB('', 0.40784314, 0.44705882, 0.49803922);
#4444=COLOUR_RGB('', 0.72549020, 0.75294118, 0.79215686);
#4445=COLOUR_RGB('', 0.31764706, 0.68627451, 0.89019608);
#4446=COLOUR_RGB('', 0.40784314, 0.44705882, 0.49803922);
#4447=COLOUR_RGB('', 0.72549020, 0.75294118, 0.79215686);
#4448=COLOUR_RGB('', 0.31764706, 0.68627451, 0.89019608);
#4449=MANIFOLD_SOLID_BREP('Heavy hex bolt 3/8-16 x 1.5',#4323);
#4450=MANIFOLD_SOLID_BREP('Part 1',#4324);
#4451=MANIFOLD_SOLID_BREP('Part 1',#4325);
#4452=MANIFOLD_SOLID_BREP('Part 1',#4326);
#4453=MANIFOLD_SOLID_BREP('Part 1',#4327);
#4454=MANIFOLD_SOLID_BREP('Part 2',#4328);
#4455=MANIFOLD_SOLID_BREP('Part 1',#4329);
#4456=MANIFOLD_SOLID_BREP('Part 4',#4330);
#4457=MANIFOLD_SOLID_BREP('Part 2',#4331);
#4458=MANIFOLD_SOLID_BREP('CRANKSHAFT',#4332);
#4459=MANIFOLD_SOLID_BREP('Part 3',#4333);
#4460=SHAPE_DEFINITION_REPRESENTATION(#8562,#4472);
#4461=SHAPE_DEFINITION_REPRESENTATION(#8563,#4473);
#4462=SHAPE_DEFINITION_REPRESENTATION(#8565,#4474);
#4463=SHAPE_DEFINITION_REPRESENTATION(#8567,#4475);
#4464=SHAPE_DEFINITION_REPRESENTATION(#8569,#4476);
#4465=SHAPE_DEFINITION_REPRESENTATION(#8573,#4477);
#4466=SHAPE_DEFINITION_REPRESENTATION(#8575,#4478);
#4467=SHAPE_DEFINITION_REPRESENTATION(#8578,#4479);
#4468=SHAPE_DEFINITION_REPRESENTATION(#8580,#4480);
#4469=SHAPE_DEFINITION_REPRESENTATION(#8582,#4481);
#4470=SHAPE_DEFINITION_REPRESENTATION(#8584,#4482);
#4471=SHAPE_DEFINITION_REPRESENTATION(#8586,#4483);
#4472=SHAPE_REPRESENTATION('MAS-680',(#4484,#4513,#4522,#4533,#4585,
#4586,#4587,#4596,#4649,#4650,#4940,#4951,#4960,#5051,#5062,#5063),#8535);
#4473=SHAPE_REPRESENTATION('Heavy hex bolt 3/8-16 x 1.5',(#4484),#8536);
#4474=SHAPE_REPRESENTATION('Part 1',(#4484),#8537);
#4475=SHAPE_REPRESENTATION('Part 1',(#4484),#8538);
#4476=SHAPE_REPRESENTATION('Part 1',(#4484),#8539);
#4477=SHAPE_REPRESENTATION('Part 1',(#4484),#8540);
#4478=SHAPE_REPRESENTATION('Part 2',(#4484),#8541);
#4479=SHAPE_REPRESENTATION('Part 1',(#4484),#8542);
#4480=SHAPE_REPRESENTATION('Part 4',(#4484),#8543);
#4481=SHAPE_REPRESENTATION('Part 2',(#4484),#8544);
#4482=SHAPE_REPRESENTATION('CRANKSHAFT',(#4484),#8545);
#4483=SHAPE_REPRESENTATION('Part 3',(#4484),#8546);
#4484=AXIS2_PLACEMENT_3D('',#6402,#5064,#5065);
#4485=AXIS2_PLACEMENT_3D('',#6403,#5066,#5067);
#4486=AXIS2_PLACEMENT_3D('',#6420,#5071,#5072);
#4487=AXIS2_PLACEMENT_3D('',#6434,#5075,#5076);
#4488=AXIS2_PLACEMENT_3D('',#6448,#5079,#5080);
#4489=AXIS2_PLACEMENT_3D('',#6462,#5083,#5084);
#4490=AXIS2_PLACEMENT_3D('',#6476,#5087,#5088);
#4491=AXIS2_PLACEMENT_3D('',#6487,#5090,#5091);
#4492=AXIS2_PLACEMENT_3D('',#6488,#5092,#5093);
#4493=AXIS2_PLACEMENT_3D('',#6490,#5094,#5095);
#4494=AXIS2_PLACEMENT_3D('',#6491,#5096,#5097);
#4495=AXIS2_PLACEMENT_3D('',#6493,#5098,#5099);
#4496=AXIS2_PLACEMENT_3D('',#6495,#5100,#5101);
#4497=AXIS2_PLACEMENT_3D('',#6496,#5102,#5103);
#4498=AXIS2_PLACEMENT_3D('',#6498,#5104,#5105);
#4499=AXIS2_PLACEMENT_3D('',#6499,#5106,#5107);
#4500=AXIS2_PLACEMENT_3D('',#6500,#5108,#5109);
#4501=AXIS2_PLACEMENT_3D('',#6501,#5110,#5111);
#4502=AXIS2_PLACEMENT_3D('',#6502,#5112,#5113);
#4503=AXIS2_PLACEMENT_3D('',#6503,#5114,#5115);
#4504=AXIS2_PLACEMENT_3D('',#6504,#5116,#5117);
#4505=AXIS2_PLACEMENT_3D('',#6505,#5118,#5119);
#4506=AXIS2_PLACEMENT_3D('',#6506,#5120,#5121);
#4507=AXIS2_PLACEMENT_3D('',#6507,#5122,#5123);
#4508=AXIS2_PLACEMENT_3D('',#6508,#5124,#5125);
#4509=AXIS2_PLACEMENT_3D('',#6509,#5126,#5127);
#4510=AXIS2_PLACEMENT_3D('',#6510,#5128,#5129);
#4511=AXIS2_PLACEMENT_3D('',#6511,#5130,#5131);
#4512=AXIS2_PLACEMENT_3D('',#6512,#5132,#5133);
#4513=AXIS2_PLACEMENT_3D('',#6513,#5134,#5135);
#4514=AXIS2_PLACEMENT_3D('',#6514,#5136,#5137);
#4515=AXIS2_PLACEMENT_3D('',#6515,#5138,#5139);
#4516=AXIS2_PLACEMENT_3D('',#6517,#5140,#5141);
#4517=AXIS2_PLACEMENT_3D('',#6519,#5142,#5143);
#4518=AXIS2_PLACEMENT_3D('',#6520,#5144,#5145);
#4519=AXIS2_PLACEMENT_3D('',#6522,#5146,#5147);
#4520=AXIS2_PLACEMENT_3D('',#6524,#5148,#5149);
#4521=AXIS2_PLACEMENT_3D('',#6525,#5150,#5151);
#4522=AXIS2_PLACEMENT_3D('',#6526,#5152,#5153);
#4523=AXIS2_PLACEMENT_3D('',#6527,#5154,#5155);
#4524=AXIS2_PLACEMENT_3D('',#6528,#5156,#5157);
#4525=AXIS2_PLACEMENT_3D('',#6533,#5159,#5160);
#4526=AXIS2_PLACEMENT_3D('',#6536,#5162,#5163);
#4527=AXIS2_PLACEMENT_3D('',#6542,#5167,#5168);
#4528=AXIS2_PLACEMENT_3D('',#6543,#5169,#5170);
#4529=AXIS2_PLACEMENT_3D('',#6547,#5172,#5173);
#4530=AXIS2_PLACEMENT_3D('',#6548,#5174,#5175);
#4531=AXIS2_PLACEMENT_3D('',#6551,#5178,#5179);
#4532=AXIS2_PLACEMENT_3D('',#6552,#5180,#5181);
#4533=AXIS2_PLACEMENT_3D('',#6553,#5182,#5183);
#4534=AXIS2_PLACEMENT_3D('',#6554,#5184,#5185);
#4535=AXIS2_PLACEMENT_3D('',#6575,#5186,#5187);
#4536=AXIS2_PLACEMENT_3D('',#6577,#5188,#5189);
#4537=AXIS2_PLACEMENT_3D('',#6600,#5190,#5191);
#4538=AXIS2_PLACEMENT_3D('',#6602,#5192,#5193);
#4539=AXIS2_PLACEMENT_3D('',#6626,#5194,#5195);
#4540=AXIS2_PLACEMENT_3D('',#6627,#5196,#5197);
#4541=AXIS2_PLACEMENT_3D('',#6649,#5198,#5199);
#4542=AXIS2_PLACEMENT_3D('',#6651,#5200,#5201);
#4543=AXIS2_PLACEMENT_3D('',#6652,#5202,#5203);
#4544=AXIS2_PLACEMENT_3D('',#6654,#5204,#5205);
#4545=AXIS2_PLACEMENT_3D('',#6655,#5206,#5207);
#4546=AXIS2_PLACEMENT_3D('',#6657,#5208,#5209);
#4547=AXIS2_PLACEMENT_3D('',#6658,#5210,#5211);
#4548=AXIS2_PLACEMENT_3D('',#6660,#5212,#5213);
#4549=AXIS2_PLACEMENT_3D('',#6661,#5214,#5215);
#4550=AXIS2_PLACEMENT_3D('',#6663,#5216,#5217);
#4551=AXIS2_PLACEMENT_3D('',#6664,#5218,#5219);
#4552=AXIS2_PLACEMENT_3D('',#6666,#5220,#5221);
#4553=AXIS2_PLACEMENT_3D('',#6667,#5222,#5223);
#4554=AXIS2_PLACEMENT_3D('',#6669,#5224,#5225);
#4555=AXIS2_PLACEMENT_3D('',#6670,#5226,#5227);
#4556=AXIS2_PLACEMENT_3D('',#6672,#5228,#5229);
#4557=AXIS2_PLACEMENT_3D('',#6673,#5230,#5231);
#4558=AXIS2_PLACEMENT_3D('',#6675,#5232,#5233);
#4559=AXIS2_PLACEMENT_3D('',#6676,#5234,#5235);
#4560=AXIS2_PLACEMENT_3D('',#6678,#5236,#5237);
#4561=AXIS2_PLACEMENT_3D('',#6679,#5238,#5239);
#4562=AXIS2_PLACEMENT_3D('',#6681,#5240,#5241);
#4563=AXIS2_PLACEMENT_3D('',#6682,#5242,#5243);
#4564=AXIS2_PLACEMENT_3D('',#6684,#5244,#5245);
#4565=AXIS2_PLACEMENT_3D('',#6685,#5246,#5247);
#4566=AXIS2_PLACEMENT_3D('',#6687,#5248,#5249);
#4567=AXIS2_PLACEMENT_3D('',#6688,#5250,#5251);
#4568=AXIS2_PLACEMENT_3D('',#6690,#5252,#5253);
#4569=AXIS2_PLACEMENT_3D('',#6691,#5254,#5255);
#4570=AXIS2_PLACEMENT_3D('',#6693,#5256,#5257);
#4571=AXIS2_PLACEMENT_3D('',#6694,#5258,#5259);
#4572=AXIS2_PLACEMENT_3D('',#6696,#5260,#5261);
#4573=AXIS2_PLACEMENT_3D('',#6697,#5262,#5263);
#4574=AXIS2_PLACEMENT_3D('',#6699,#5264,#5265);
#4575=AXIS2_PLACEMENT_3D('',#6700,#5266,#5267);
#4576=AXIS2_PLACEMENT_3D('',#6701,#5268,#5269);
#4577=AXIS2_PLACEMENT_3D('',#6702,#5270,#5271);
#4578=AXIS2_PLACEMENT_3D('',#6703,#5272,#5273);
#4579=AXIS2_PLACEMENT_3D('',#6705,#5274,#5275);
#4580=AXIS2_PLACEMENT_3D('',#6706,#5276,#5277);
#4581=AXIS2_PLACEMENT_3D('',#6707,#5278,#5279);
#4582=AXIS2_PLACEMENT_3D('',#6709,#5280,#5281);
#4583=AXIS2_PLACEMENT_3D('',#6710,#5282,#5283);
#4584=AXIS2_PLACEMENT_3D('',#6712,#5284,#5285);
#4585=AXIS2_PLACEMENT_3D('',#6713,#5286,#5287);
#4586=AXIS2_PLACEMENT_3D('',#6714,#5288,#5289);
#4587=AXIS2_PLACEMENT_3D('',#6715,#5290,#5291);
#4588=AXIS2_PLACEMENT_3D('',#6716,#5292,#5293);
#4589=AXIS2_PLACEMENT_3D('',#6717,#5294,#5295);
#4590=AXIS2_PLACEMENT_3D('',#6719,#5296,#5297);
#4591=AXIS2_PLACEMENT_3D('',#6721,#5298,#5299);
#4592=AXIS2_PLACEMENT_3D('',#6722,#5300,#5301);
#4593=AXIS2_PLACEMENT_3D('',#6724,#5302,#5303);
#4594=AXIS2_PLACEMENT_3D('',#6726,#5304,#5305);
#4595=AXIS2_PLACEMENT_3D('',#6727,#5306,#5307);
#4596=AXIS2_PLACEMENT_3D('',#6728,#5308,#5309);
#4597=AXIS2_PLACEMENT_3D('',#6729,#5310,#5311);
#4598=AXIS2_PLACEMENT_3D('',#6733,#5313,#5314);
#4599=AXIS2_PLACEMENT_3D('',#6737,#5316,#5317);
#4600=AXIS2_PLACEMENT_3D('',#6738,#5318,#5319);
#4601=AXIS2_PLACEMENT_3D('',#6745,#5320,#5321);
#4602=AXIS2_PLACEMENT_3D('',#6752,#5322,#5323);
#4603=AXIS2_PLACEMENT_3D('',#6765,#5324,#5325);
#4604=AXIS2_PLACEMENT_3D('',#6766,#5326,#5327);
#4605=AXIS2_PLACEMENT_3D('',#6767,#5328,#5329);
#4606=AXIS2_PLACEMENT_3D('',#6772,#5332,#5333);
#4607=AXIS2_PLACEMENT_3D('',#6773,#5334,#5335);
#4608=AXIS2_PLACEMENT_3D('',#6778,#5338,#5339);
#4609=AXIS2_PLACEMENT_3D('',#6781,#5341,#5342);
#4610=AXIS2_PLACEMENT_3D('',#6784,#5344,#5345);
#4611=AXIS2_PLACEMENT_3D('',#6787,#5347,#5348);
#4612=AXIS2_PLACEMENT_3D('',#6790,#5350,#5351);
#4613=AXIS2_PLACEMENT_3D('',#6791,#5352,#5353);
#4614=AXIS2_PLACEMENT_3D('',#6796,#5356,#5357);
#4615=AXIS2_PLACEMENT_3D('',#6797,#5358,#5359);
#4616=AXIS2_PLACEMENT_3D('',#6802,#5362,#5363);
#4617=AXIS2_PLACEMENT_3D('',#6805,#5366,#5367);
#4618=AXIS2_PLACEMENT_3D('',#6809,#5369,#5370);
#4619=AXIS2_PLACEMENT_3D('',#6813,#5372,#5373);
#4620=AXIS2_PLACEMENT_3D('',#6814,#5374,#5375);
#4621=AXIS2_PLACEMENT_3D('',#6815,#5376,#5377);
#4622=AXIS2_PLACEMENT_3D('',#6824,#5378,#5379);
#4623=AXIS2_PLACEMENT_3D('',#6831,#5380,#5381);
#4624=AXIS2_PLACEMENT_3D('',#6834,#5384,#5385);
#4625=AXIS2_PLACEMENT_3D('',#6835,#5386,#5387);
#4626=AXIS2_PLACEMENT_3D('',#6844,#5388,#5389);
#4627=AXIS2_PLACEMENT_3D('',#6851,#5390,#5391);
#4628=AXIS2_PLACEMENT_3D('',#6855,#5393,#5394);
#4629=AXIS2_PLACEMENT_3D('',#6859,#5396,#5397);
#4630=AXIS2_PLACEMENT_3D('',#6860,#5398,#5399);
#4631=AXIS2_PLACEMENT_3D('',#6863,#5402,#5403);
#4632=AXIS2_PLACEMENT_3D('',#6866,#5406,#5407);
#4633=AXIS2_PLACEMENT_3D('',#6867,#5408,#5409);
#4634=AXIS2_PLACEMENT_3D('',#6872,#5412,#5413);
#4635=AXIS2_PLACEMENT_3D('',#6873,#5414,#5415);
#4636=AXIS2_PLACEMENT_3D('',#6878,#5418,#5419);
#4637=AXIS2_PLACEMENT_3D('',#6881,#5422,#5423);
#4638=AXIS2_PLACEMENT_3D('',#6884,#5426,#5427);
#4639=AXIS2_PLACEMENT_3D('',#6887,#5430,#5431);
#4640=AXIS2_PLACEMENT_3D('',#6888,#5432,#5433);
#4641=AXIS2_PLACEMENT_3D('',#6890,#5434,#5435);
#4642=AXIS2_PLACEMENT_3D('',#6891,#5436,#5437);
#4643=AXIS2_PLACEMENT_3D('',#6893,#5438,#5439);
#4644=AXIS2_PLACEMENT_3D('',#6894,#5440,#5441);
#4645=AXIS2_PLACEMENT_3D('',#6896,#5442,#5443);
#4646=AXIS2_PLACEMENT_3D('',#6897,#5444,#5445);
#4647=AXIS2_PLACEMENT_3D('',#6899,#5446,#5447);
#4648=AXIS2_PLACEMENT_3D('',#6900,#5448,#5449);
#4649=AXIS2_PLACEMENT_3D('',#6901,#5450,#5451);
#4650=AXIS2_PLACEMENT_3D('',#6902,#5452,#5453);
#4651=AXIS2_PLACEMENT_3D('',#6903,#5454,#5455);
#4652=AXIS2_PLACEMENT_3D('',#6909,#5458,#5459);
#4653=AXIS2_PLACEMENT_3D('',#6915,#5462,#5463);
#4654=AXIS2_PLACEMENT_3D('',#6917,#5464,#5465);
#4655=AXIS2_PLACEMENT_3D('',#6919,#5466,#5467);
#4656=AXIS2_PLACEMENT_3D('',#6920,#5468,#5469);
#4657=AXIS2_PLACEMENT_3D('',#6926,#5472,#5473);
#4658=AXIS2_PLACEMENT_3D('',#6928,#5474,#5475);
#4659=AXIS2_PLACEMENT_3D('',#6930,#5476,#5477);
#4660=AXIS2_PLACEMENT_3D('',#6936,#5480,#5481);
#4661=AXIS2_PLACEMENT_3D('',#6937,#5482,#5483);
#4662=AXIS2_PLACEMENT_3D('',#6946,#5488,#5489);
#4663=AXIS2_PLACEMENT_3D('',#6955,#5494,#5495);
#4664=AXIS2_PLACEMENT_3D('',#6959,#5497,#5498);
#4665=AXIS2_PLACEMENT_3D('',#6963,#5500,#5501);
#4666=AXIS2_PLACEMENT_3D('',#6964,#5502,#5503);
#4667=AXIS2_PLACEMENT_3D('',#6985,#5504,#5505);
#4668=AXIS2_PLACEMENT_3D('',#6987,#5506,#5507);
#4669=AXIS2_PLACEMENT_3D('',#7008,#5508,#5509);
#4670=AXIS2_PLACEMENT_3D('',#7010,#5510,#5511);
#4671=AXIS2_PLACEMENT_3D('',#7014,#5513,#5514);
#4672=AXIS2_PLACEMENT_3D('',#7018,#5516,#5517);
#4673=AXIS2_PLACEMENT_3D('',#7019,#5518,#5519);
#4674=AXIS2_PLACEMENT_3D('',#7022,#5522,#5523);
#4675=AXIS2_PLACEMENT_3D('',#7023,#5524,#5525);
#4676=AXIS2_PLACEMENT_3D('',#7028,#5527,#5528);
#4677=AXIS2_PLACEMENT_3D('',#7031,#5530,#5531);
#4678=AXIS2_PLACEMENT_3D('',#7034,#5534,#5535);
#4679=AXIS2_PLACEMENT_3D('',#7035,#5536,#5537);
#4680=AXIS2_PLACEMENT_3D('',#7036,#5538,#5539);
#4681=AXIS2_PLACEMENT_3D('',#7037,#5540,#5541);
#4682=AXIS2_PLACEMENT_3D('',#7038,#5542,#5543);
#4683=AXIS2_PLACEMENT_3D('',#7039,#5544,#5545);
#4684=AXIS2_PLACEMENT_3D('',#7040,#5546,#5547);
#4685=AXIS2_PLACEMENT_3D('',#7041,#5548,#5549);
#4686=AXIS2_PLACEMENT_3D('',#7042,#5550,#5551);
#4687=AXIS2_PLACEMENT_3D('',#7043,#5552,#5553);
#4688=AXIS2_PLACEMENT_3D('',#7044,#5554,#5555);
#4689=AXIS2_PLACEMENT_3D('',#7045,#5556,#5557);
#4690=AXIS2_PLACEMENT_3D('',#7046,#5558,#5559);
#4691=AXIS2_PLACEMENT_3D('',#7057,#5560,#5561);
#4692=AXIS2_PLACEMENT_3D('',#7068,#5562,#5563);
#4693=AXIS2_PLACEMENT_3D('',#7072,#5565,#5566);
#4694=AXIS2_PLACEMENT_3D('',#7074,#5567,#5568);
#4695=AXIS2_PLACEMENT_3D('',#7076,#5569,#5570);
#4696=AXIS2_PLACEMENT_3D('',#7080,#5572,#5573);
#4697=AXIS2_PLACEMENT_3D('',#7082,#5574,#5575);
#4698=AXIS2_PLACEMENT_3D('',#7084,#5576,#5577);
#4699=AXIS2_PLACEMENT_3D('',#7085,#5578,#5579);
#4700=AXIS2_PLACEMENT_3D('',#7089,#5581,#5582);
#4701=AXIS2_PLACEMENT_3D('',#7091,#5583,#5584);
#4702=AXIS2_PLACEMENT_3D('',#7093,#5585,#5586);
#4703=AXIS2_PLACEMENT_3D('',#7097,#5588,#5589);
#4704=AXIS2_PLACEMENT_3D('',#7099,#5590,#5591);
#4705=AXIS2_PLACEMENT_3D('',#7101,#5592,#5593);
#4706=AXIS2_PLACEMENT_3D('',#7102,#5594,#5595);
#4707=AXIS2_PLACEMENT_3D('',#7103,#5596,#5597);
#4708=AXIS2_PLACEMENT_3D('',#7106,#5598,#5599);
#4709=AXIS2_PLACEMENT_3D('',#7110,#5601,#5602);
#4710=AXIS2_PLACEMENT_3D('',#7112,#5603,#5604);
#4711=AXIS2_PLACEMENT_3D('',#7114,#5605,#5606);
#4712=AXIS2_PLACEMENT_3D('',#7115,#5607,#5608);
#4713=AXIS2_PLACEMENT_3D('',#7117,#5609,#5610);
#4714=AXIS2_PLACEMENT_3D('',#7121,#5612,#5613);
#4715=AXIS2_PLACEMENT_3D('',#7131,#5614,#5615);
#4716=AXIS2_PLACEMENT_3D('',#7135,#5617,#5618);
#4717=AXIS2_PLACEMENT_3D('',#7145,#5619,#5620);
#4718=AXIS2_PLACEMENT_3D('',#7146,#5621,#5622);
#4719=AXIS2_PLACEMENT_3D('',#7156,#5623,#5624);
#4720=AXIS2_PLACEMENT_3D('',#7160,#5626,#5627);
#4721=AXIS2_PLACEMENT_3D('',#7170,#5628,#5629);
#4722=AXIS2_PLACEMENT_3D('',#7174,#5631,#5632);
#4723=AXIS2_PLACEMENT_3D('',#7175,#5633,#5634);
#4724=AXIS2_PLACEMENT_3D('',#7176,#5635,#5636);
#4725=AXIS2_PLACEMENT_3D('',#7179,#5637,#5638);
#4726=AXIS2_PLACEMENT_3D('',#7183,#5640,#5641);
#4727=AXIS2_PLACEMENT_3D('',#7185,#5642,#5643);
#4728=AXIS2_PLACEMENT_3D('',#7187,#5644,#5645);
#4729=AXIS2_PLACEMENT_3D('',#7188,#5646,#5647);
#4730=AXIS2_PLACEMENT_3D('',#7190,#5648,#5649);
#4731=AXIS2_PLACEMENT_3D('',#7194,#5651,#5652);
#4732=AXIS2_PLACEMENT_3D('',#7196,#5653,#5654);
#4733=AXIS2_PLACEMENT_3D('',#7198,#5655,#5656);
#4734=AXIS2_PLACEMENT_3D('',#7202,#5658,#5659);
#4735=AXIS2_PLACEMENT_3D('',#7204,#5660,#5661);
#4736=AXIS2_PLACEMENT_3D('',#7206,#5662,#5663);
#4737=AXIS2_PLACEMENT_3D('',#7207,#5664,#5665);
#4738=AXIS2_PLACEMENT_3D('',#7211,#5667,#5668);
#4739=AXIS2_PLACEMENT_3D('',#7213,#5669,#5670);
#4740=AXIS2_PLACEMENT_3D('',#7215,#5671,#5672);
#4741=AXIS2_PLACEMENT_3D('',#7219,#5674,#5675);
#4742=AXIS2_PLACEMENT_3D('',#7221,#5676,#5677);
#4743=AXIS2_PLACEMENT_3D('',#7223,#5678,#5679);
#4744=AXIS2_PLACEMENT_3D('',#7224,#5680,#5681);
#4745=AXIS2_PLACEMENT_3D('',#7225,#5682,#5683);
#4746=AXIS2_PLACEMENT_3D('',#7230,#5685,#5686);
#4747=AXIS2_PLACEMENT_3D('',#7238,#5687,#5688);
#4748=AXIS2_PLACEMENT_3D('',#7242,#5690,#5691);
#4749=AXIS2_PLACEMENT_3D('',#7249,#5692,#5693);
#4750=AXIS2_PLACEMENT_3D('',#7250,#5694,#5695);
#4751=AXIS2_PLACEMENT_3D('',#7251,#5696,#5697);
#4752=AXIS2_PLACEMENT_3D('',#7252,#5698,#5699);
#4753=AXIS2_PLACEMENT_3D('',#7253,#5700,#5701);
#4754=AXIS2_PLACEMENT_3D('',#7258,#5703,#5704);
#4755=AXIS2_PLACEMENT_3D('',#7266,#5705,#5706);
#4756=AXIS2_PLACEMENT_3D('',#7270,#5708,#5709);
#4757=AXIS2_PLACEMENT_3D('',#7277,#5710,#5711);
#4758=AXIS2_PLACEMENT_3D('',#7280,#5714,#5715);
#4759=AXIS2_PLACEMENT_3D('',#7283,#5718,#5719);
#4760=AXIS2_PLACEMENT_3D('',#7284,#5720,#5721);
#4761=AXIS2_PLACEMENT_3D('',#7286,#5722,#5723);
#4762=AXIS2_PLACEMENT_3D('',#7288,#5724,#5725);
#4763=AXIS2_PLACEMENT_3D('',#7297,#5730,#5731);
#4764=AXIS2_PLACEMENT_3D('',#7304,#5732,#5733);
#4765=AXIS2_PLACEMENT_3D('',#7305,#5734,#5735);
#4766=AXIS2_PLACEMENT_3D('',#7309,#5737,#5738);
#4767=AXIS2_PLACEMENT_3D('',#7320,#5739,#5740);
#4768=AXIS2_PLACEMENT_3D('',#7326,#5744,#5745);
#4769=AXIS2_PLACEMENT_3D('',#7327,#5746,#5747);
#4770=AXIS2_PLACEMENT_3D('',#7334,#5748,#5749);
#4771=AXIS2_PLACEMENT_3D('',#7335,#5750,#5751);
#4772=AXIS2_PLACEMENT_3D('',#7336,#5752,#5753);
#4773=AXIS2_PLACEMENT_3D('',#7340,#5755,#5756);
#4774=AXIS2_PLACEMENT_3D('',#7344,#5758,#5759);
#4775=AXIS2_PLACEMENT_3D('',#7345,#5760,#5761);
#4776=AXIS2_PLACEMENT_3D('',#7354,#5766,#5767);
#4777=AXIS2_PLACEMENT_3D('',#7358,#5769,#5770);
#4778=AXIS2_PLACEMENT_3D('',#7365,#5771,#5772);
#4779=AXIS2_PLACEMENT_3D('',#7366,#5773,#5774);
#4780=AXIS2_PLACEMENT_3D('',#7367,#5775,#5776);
#4781=AXIS2_PLACEMENT_3D('',#7373,#5780,#5781);
#4782=AXIS2_PLACEMENT_3D('',#7380,#5782,#5783);
#4783=AXIS2_PLACEMENT_3D('',#7381,#5784,#5785);
#4784=AXIS2_PLACEMENT_3D('',#7382,#5786,#5787);
#4785=AXIS2_PLACEMENT_3D('',#7393,#5788,#5789);
#4786=AXIS2_PLACEMENT_3D('',#7397,#5791,#5792);
#4787=AXIS2_PLACEMENT_3D('',#7401,#5794,#5795);
#4788=AXIS2_PLACEMENT_3D('',#7402,#5796,#5797);
#4789=AXIS2_PLACEMENT_3D('',#7409,#5798,#5799);
#4790=AXIS2_PLACEMENT_3D('',#7422,#5800,#5801);
#4791=AXIS2_PLACEMENT_3D('',#7434,#5803,#5804);
#4792=AXIS2_PLACEMENT_3D('',#7442,#5805,#5806);
#4793=AXIS2_PLACEMENT_3D('',#7448,#5807,#5808);
#4794=AXIS2_PLACEMENT_3D('',#7455,#5809,#5810);
#4795=AXIS2_PLACEMENT_3D('',#7468,#5811,#5812);
#4796=AXIS2_PLACEMENT_3D('',#7480,#5814,#5815);
#4797=AXIS2_PLACEMENT_3D('',#7488,#5816,#5817);
#4798=AXIS2_PLACEMENT_3D('',#7494,#5818,#5819);
#4799=AXIS2_PLACEMENT_3D('',#7501,#5820,#5821);
#4800=AXIS2_PLACEMENT_3D('',#7512,#5822,#5823);
#4801=AXIS2_PLACEMENT_3D('',#7519,#5824,#5825);
#4802=AXIS2_PLACEMENT_3D('',#7530,#5826,#5827);
#4803=AXIS2_PLACEMENT_3D('',#7541,#5828,#5829);
#4804=AXIS2_PLACEMENT_3D('',#7547,#5830,#5831);
#4805=AXIS2_PLACEMENT_3D('',#7553,#5832,#5833);
#4806=AXIS2_PLACEMENT_3D('',#7554,#5834,#5835);
#4807=AXIS2_PLACEMENT_3D('',#7555,#5836,#5837);
#4808=AXIS2_PLACEMENT_3D('',#7557,#5838,#5839);
#4809=AXIS2_PLACEMENT_3D('',#7559,#5840,#5841);
#4810=AXIS2_PLACEMENT_3D('',#7560,#5842,#5843);
#4811=AXIS2_PLACEMENT_3D('',#7562,#5844,#5845);
#4812=AXIS2_PLACEMENT_3D('',#7564,#5846,#5847);
#4813=AXIS2_PLACEMENT_3D('',#7565,#5848,#5849);
#4814=AXIS2_PLACEMENT_3D('',#7571,#5850,#5851);
#4815=AXIS2_PLACEMENT_3D('',#7589,#5852,#5853);
#4816=AXIS2_PLACEMENT_3D('',#7590,#5854,#5855);
#4817=AXIS2_PLACEMENT_3D('',#7591,#5856,#5857);
#4818=AXIS2_PLACEMENT_3D('',#7592,#5858,#5859);
#4819=AXIS2_PLACEMENT_3D('',#7621,#5860,#5861);
#4820=AXIS2_PLACEMENT_3D('',#7627,#5862,#5863);
#4821=AXIS2_PLACEMENT_3D('',#7633,#5864,#5865);
#4822=AXIS2_PLACEMENT_3D('',#7634,#5866,#5867);
#4823=AXIS2_PLACEMENT_3D('',#7653,#5868,#5869);
#4824=AXIS2_PLACEMENT_3D('',#7654,#5870,#5871);
#4825=AXIS2_PLACEMENT_3D('',#7655,#5872,#5873);
#4826=AXIS2_PLACEMENT_3D('',#7671,#5874,#5875);
#4827=AXIS2_PLACEMENT_3D('',#7672,#5876,#5877);
#4828=AXIS2_PLACEMENT_3D('',#7673,#5878,#5879);
#4829=AXIS2_PLACEMENT_3D('',#7674,#5880,#5881);
#4830=AXIS2_PLACEMENT_3D('',#7675,#5882,#5883);
#4831=AXIS2_PLACEMENT_3D('',#7676,#5884,#5885);
#4832=AXIS2_PLACEMENT_3D('',#7677,#5886,#5887);
#4833=AXIS2_PLACEMENT_3D('',#7678,#5888,#5889);
#4834=AXIS2_PLACEMENT_3D('',#7700,#5890,#5891);
#4835=AXIS2_PLACEMENT_3D('',#7701,#5892,#5893);
#4836=AXIS2_PLACEMENT_3D('',#7702,#5894,#5895);
#4837=AXIS2_PLACEMENT_3D('',#7703,#5896,#5897);
#4838=AXIS2_PLACEMENT_3D('',#7719,#5898,#5899);
#4839=AXIS2_PLACEMENT_3D('',#7720,#5900,#5901);
#4840=AXIS2_PLACEMENT_3D('',#7721,#5902,#5903);
#4841=AXIS2_PLACEMENT_3D('',#7722,#5904,#5905);
#4842=AXIS2_PLACEMENT_3D('',#7723,#5906,#5907);
#4843=AXIS2_PLACEMENT_3D('',#7724,#5908,#5909);
#4844=AXIS2_PLACEMENT_3D('',#7725,#5910,#5911);
#4845=AXIS2_PLACEMENT_3D('',#7726,#5912,#5913);
#4846=AXIS2_PLACEMENT_3D('',#7748,#5914,#5915);
#4847=AXIS2_PLACEMENT_3D('',#7749,#5916,#5917);
#4848=AXIS2_PLACEMENT_3D('',#7750,#5918,#5919);
#4849=AXIS2_PLACEMENT_3D('',#7756,#5920,#5921);
#4850=AXIS2_PLACEMENT_3D('',#7774,#5922,#5923);
#4851=AXIS2_PLACEMENT_3D('',#7775,#5924,#5925);
#4852=AXIS2_PLACEMENT_3D('',#7776,#5926,#5927);
#4853=AXIS2_PLACEMENT_3D('',#7777,#5928,#5929);
#4854=AXIS2_PLACEMENT_3D('',#7806,#5930,#5931);
#4855=AXIS2_PLACEMENT_3D('',#7812,#5932,#5933);
#4856=AXIS2_PLACEMENT_3D('',#7818,#5934,#5935);
#4857=AXIS2_PLACEMENT_3D('',#7819,#5936,#5937);
#4858=AXIS2_PLACEMENT_3D('',#7838,#5938,#5939);
#4859=AXIS2_PLACEMENT_3D('',#7839,#5940,#5941);
#4860=AXIS2_PLACEMENT_3D('',#7840,#5942,#5943);
#4861=AXIS2_PLACEMENT_3D('',#7856,#5944,#5945);
#4862=AXIS2_PLACEMENT_3D('',#7857,#5946,#5947);
#4863=AXIS2_PLACEMENT_3D('',#7858,#5948,#5949);
#4864=AXIS2_PLACEMENT_3D('',#7859,#5950,#5951);
#4865=AXIS2_PLACEMENT_3D('',#7860,#5952,#5953);
#4866=AXIS2_PLACEMENT_3D('',#7861,#5954,#5955);
#4867=AXIS2_PLACEMENT_3D('',#7862,#5956,#5957);
#4868=AXIS2_PLACEMENT_3D('',#7863,#5958,#5959);
#4869=AXIS2_PLACEMENT_3D('',#7885,#5960,#5961);
#4870=AXIS2_PLACEMENT_3D('',#7886,#5962,#5963);
#4871=AXIS2_PLACEMENT_3D('',#7887,#5964,#5965);
#4872=AXIS2_PLACEMENT_3D('',#7888,#5966,#5967);
#4873=AXIS2_PLACEMENT_3D('',#7904,#5968,#5969);
#4874=AXIS2_PLACEMENT_3D('',#7905,#5970,#5971);
#4875=AXIS2_PLACEMENT_3D('',#7906,#5972,#5973);
#4876=AXIS2_PLACEMENT_3D('',#7907,#5974,#5975);
#4877=AXIS2_PLACEMENT_3D('',#7908,#5976,#5977);
#4878=AXIS2_PLACEMENT_3D('',#7909,#5978,#5979);
#4879=AXIS2_PLACEMENT_3D('',#7910,#5980,#5981);
#4880=AXIS2_PLACEMENT_3D('',#7911,#5982,#5983);
#4881=AXIS2_PLACEMENT_3D('',#7933,#5984,#5985);
#4882=AXIS2_PLACEMENT_3D('',#7934,#5986,#5987);
#4883=AXIS2_PLACEMENT_3D('',#7945,#5988,#5989);
#4884=AXIS2_PLACEMENT_3D('',#7951,#5990,#5991);
#4885=AXIS2_PLACEMENT_3D('',#7957,#5992,#5993);
#4886=AXIS2_PLACEMENT_3D('',#7958,#5994,#5995);
#4887=AXIS2_PLACEMENT_3D('',#7959,#5996,#5997);
#4888=AXIS2_PLACEMENT_3D('',#7960,#5998,#5999);
#4889=AXIS2_PLACEMENT_3D('',#7961,#6000,#6001);
#4890=AXIS2_PLACEMENT_3D('',#7962,#6002,#6003);
#4891=AXIS2_PLACEMENT_3D('',#7963,#6004,#6005);
#4892=AXIS2_PLACEMENT_3D('',#7964,#6006,#6007);
#4893=AXIS2_PLACEMENT_3D('',#7965,#6008,#6009);
#4894=AXIS2_PLACEMENT_3D('',#7966,#6010,#6011);
#4895=AXIS2_PLACEMENT_3D('',#7967,#6012,#6013);
#4896=AXIS2_PLACEMENT_3D('',#7968,#6014,#6015);
#4897=AXIS2_PLACEMENT_3D('',#7969,#6016,#6017);
#4898=AXIS2_PLACEMENT_3D('',#7970,#6018,#6019);
#4899=AXIS2_PLACEMENT_3D('',#7971,#6020,#6021);
#4900=AXIS2_PLACEMENT_3D('',#7972,#6022,#6023);
#4901=AXIS2_PLACEMENT_3D('',#7973,#6024,#6025);
#4902=AXIS2_PLACEMENT_3D('',#7974,#6026,#6027);
#4903=AXIS2_PLACEMENT_3D('',#7975,#6028,#6029);
#4904=AXIS2_PLACEMENT_3D('',#7976,#6030,#6031);
#4905=AXIS2_PLACEMENT_3D('',#7977,#6032,#6033);
#4906=AXIS2_PLACEMENT_3D('',#7978,#6034,#6035);
#4907=AXIS2_PLACEMENT_3D('',#7979,#6036,#6037);
#4908=AXIS2_PLACEMENT_3D('',#7980,#6038,#6039);
#4909=AXIS2_PLACEMENT_3D('',#7981,#6040,#6041);
#4910=AXIS2_PLACEMENT_3D('',#7982,#6042,#6043);
#4911=AXIS2_PLACEMENT_3D('',#7983,#6044,#6045);
#4912=AXIS2_PLACEMENT_3D('',#7984,#6046,#6047);
#4913=AXIS2_PLACEMENT_3D('',#7985,#6048,#6049);
#4914=AXIS2_PLACEMENT_3D('',#7986,#6050,#6051);
#4915=AXIS2_PLACEMENT_3D('',#7987,#6052,#6053);
#4916=AXIS2_PLACEMENT_3D('',#7988,#6054,#6055);
#4917=AXIS2_PLACEMENT_3D('',#7989,#6056,#6057);
#4918=AXIS2_PLACEMENT_3D('',#7994,#6058,#6059);
#4919=AXIS2_PLACEMENT_3D('',#7999,#6060,#6061);
#4920=AXIS2_PLACEMENT_3D('',#8000,#6062,#6063);
#4921=AXIS2_PLACEMENT_3D('',#8001,#6064,#6065);
#4922=AXIS2_PLACEMENT_3D('',#8002,#6066,#6067);
#4923=AXIS2_PLACEMENT_3D('',#8003,#6068,#6069);
#4924=AXIS2_PLACEMENT_3D('',#8004,#6070,#6071);
#4925=AXIS2_PLACEMENT_3D('',#8005,#6072,#6073);
#4926=AXIS2_PLACEMENT_3D('',#8006,#6074,#6075);
#4927=AXIS2_PLACEMENT_3D('',#8007,#6076,#6077);
#4928=AXIS2_PLACEMENT_3D('',#8008,#6078,#6079);
#4929=AXIS2_PLACEMENT_3D('',#8009,#6080,#6081);
#4930=AXIS2_PLACEMENT_3D('',#8010,#6082,#6083);
#4931=AXIS2_PLACEMENT_3D('',#8011,#6084,#6085);
#4932=AXIS2_PLACEMENT_3D('',#8012,#6086,#6087);
#4933=AXIS2_PLACEMENT_3D('',#8013,#6088,#6089);
#4934=AXIS2_PLACEMENT_3D('',#8014,#6090,#6091);
#4935=AXIS2_PLACEMENT_3D('',#8019,#6092,#6093);
#4936=AXIS2_PLACEMENT_3D('',#8024,#6094,#6095);
#4937=AXIS2_PLACEMENT_3D('',#8025,#6096,#6097);
#4938=AXIS2_PLACEMENT_3D('',#8026,#6098,#6099);
#4939=AXIS2_PLACEMENT_3D('',#8027,#6100,#6101);
#4940=AXIS2_PLACEMENT_3D('',#8028,#6102,#6103);
#4941=AXIS2_PLACEMENT_3D('',#8029,#6104,#6105);
#4942=AXIS2_PLACEMENT_3D('',#8038,#6110,#6111);
#4943=AXIS2_PLACEMENT_3D('',#8039,#6112,#6113);
#4944=AXIS2_PLACEMENT_3D('',#8041,#6114,#6115);
#4945=AXIS2_PLACEMENT_3D('',#8044,#6117,#6118);
#4946=AXIS2_PLACEMENT_3D('',#8045,#6119,#6120);
#4947=AXIS2_PLACEMENT_3D('',#8049,#6122,#6123);
#4948=AXIS2_PLACEMENT_3D('',#8050,#6124,#6125);
#4949=AXIS2_PLACEMENT_3D('',#8052,#6127,#6128);
#4950=AXIS2_PLACEMENT_3D('',#8054,#6130,#6131);
#4951=AXIS2_PLACEMENT_3D('',#8055,#6132,#6133);
#4952=AXIS2_PLACEMENT_3D('',#8056,#6134,#6135);
#4953=AXIS2_PLACEMENT_3D('',#8057,#6136,#6137);
#4954=AXIS2_PLACEMENT_3D('',#8059,#6138,#6139);
#4955=AXIS2_PLACEMENT_3D('',#8061,#6140,#6141);
#4956=AXIS2_PLACEMENT_3D('',#8062,#6142,#6143);
#4957=AXIS2_PLACEMENT_3D('',#8064,#6144,#6145);
#4958=AXIS2_PLACEMENT_3D('',#8066,#6146,#6147);
#4959=AXIS2_PLACEMENT_3D('',#8067,#6148,#6149);
#4960=AXIS2_PLACEMENT_3D('',#8068,#6150,#6151);
#4961=AXIS2_PLACEMENT_3D('',#8069,#6152,#6153);
#4962=AXIS2_PLACEMENT_3D('',#8070,#6154,#6155);
#4963=AXIS2_PLACEMENT_3D('',#8072,#6156,#6157);
#4964=AXIS2_PLACEMENT_3D('',#8074,#6158,#6159);
#4965=AXIS2_PLACEMENT_3D('',#8075,#6160,#6161);
#4966=AXIS2_PLACEMENT_3D('',#8080,#6163,#6164);
#4967=AXIS2_PLACEMENT_3D('',#8084,#6166,#6167);
#4968=AXIS2_PLACEMENT_3D('',#8085,#6168,#6169);
#4969=AXIS2_PLACEMENT_3D('',#8086,#6170,#6171);
#4970=AXIS2_PLACEMENT_3D('',#8088,#6172,#6173);
#4971=AXIS2_PLACEMENT_3D('',#8090,#6174,#6175);
#4972=AXIS2_PLACEMENT_3D('',#8094,#6177,#6178);
#4973=AXIS2_PLACEMENT_3D('',#8100,#6182,#6183);
#4974=AXIS2_PLACEMENT_3D('',#8120,#6187,#6188);
#4975=AXIS2_PLACEMENT_3D('',#8123,#6190,#6191);
#4976=AXIS2_PLACEMENT_3D('',#8148,#6193,#6194);
#4977=AXIS2_PLACEMENT_3D('',#8160,#6197,#6198);
#4978=AXIS2_PLACEMENT_3D('',#8168,#6200,#6201);
#4979=AXIS2_PLACEMENT_3D('',#8170,#6203,#6204);
#4980=AXIS2_PLACEMENT_3D('',#8191,#6205,#6206);
#4981=AXIS2_PLACEMENT_3D('',#8193,#6207,#6208);
#4982=AXIS2_PLACEMENT_3D('',#8195,#6209,#6210);
#4983=AXIS2_PLACEMENT_3D('',#8197,#6212,#6213);
#4984=AXIS2_PLACEMENT_3D('',#8198,#6214,#6215);
#4985=AXIS2_PLACEMENT_3D('',#8200,#6216,#6217);
#4986=AXIS2_PLACEMENT_3D('',#8202,#6218,#6219);
#4987=AXIS2_PLACEMENT_3D('',#8203,#6220,#6221);
#4988=AXIS2_PLACEMENT_3D('',#8210,#6223,#6224);
#4989=AXIS2_PLACEMENT_3D('',#8238,#6225,#6226);
#4990=AXIS2_PLACEMENT_3D('',#8239,#6227,#6228);
#4991=AXIS2_PLACEMENT_3D('',#8241,#6230,#6231);
#4992=AXIS2_PLACEMENT_3D('',#8242,#6232,#6233);
#4993=AXIS2_PLACEMENT_3D('',#8243,#6234,#6235);
#4994=AXIS2_PLACEMENT_3D('',#8255,#6236,#6237);
#4995=AXIS2_PLACEMENT_3D('',#8256,#6238,#6239);
#4996=AXIS2_PLACEMENT_3D('',#8268,#6240,#6241);
#4997=AXIS2_PLACEMENT_3D('',#8269,#6242,#6243);
#4998=AXIS2_PLACEMENT_3D('',#8270,#6244,#6245);
#4999=AXIS2_PLACEMENT_3D('',#8272,#6246,#6247);
#5000=AXIS2_PLACEMENT_3D('',#8273,#6248,#6249);
#5001=AXIS2_PLACEMENT_3D('',#8275,#6250,#6251);
#5002=AXIS2_PLACEMENT_3D('',#8277,#6252,#6253);
#5003=AXIS2_PLACEMENT_3D('',#8279,#6254,#6255);
#5004=AXIS2_PLACEMENT_3D('',#8290,#6256,#6257);
#5005=AXIS2_PLACEMENT_3D('',#8303,#6258,#6259);
#5006=AXIS2_PLACEMENT_3D('',#8314,#6260,#6261);
#5007=AXIS2_PLACEMENT_3D('',#8315,#6262,#6263);
#5008=AXIS2_PLACEMENT_3D('',#8316,#6264,#6265);
#5009=AXIS2_PLACEMENT_3D('',#8317,#6266,#6267);
#5010=AXIS2_PLACEMENT_3D('',#8318,#6268,#6269);
#5011=AXIS2_PLACEMENT_3D('',#8319,#6270,#6271);
#5012=AXIS2_PLACEMENT_3D('',#8321,#6272,#6273);
#5013=AXIS2_PLACEMENT_3D('',#8328,#6274,#6275);
#5014=AXIS2_PLACEMENT_3D('',#8351,#6276,#6277);
#5015=AXIS2_PLACEMENT_3D('',#8352,#6278,#6279);
#5016=AXIS2_PLACEMENT_3D('',#8353,#6280,#6281);
#5017=AXIS2_PLACEMENT_3D('',#8354,#6282,#6283);
#5018=AXIS2_PLACEMENT_3D('',#8358,#6285,#6286);
#5019=AXIS2_PLACEMENT_3D('',#8364,#6290,#6291);
#5020=AXIS2_PLACEMENT_3D('',#8365,#6292,#6293);
#5021=AXIS2_PLACEMENT_3D('',#8367,#6294,#6295);
#5022=AXIS2_PLACEMENT_3D('',#8368,#6296,#6297);
#5023=AXIS2_PLACEMENT_3D('',#8369,#6298,#6299);
#5024=AXIS2_PLACEMENT_3D('',#8370,#6300,#6301);
#5025=AXIS2_PLACEMENT_3D('',#8372,#6302,#6303);
#5026=AXIS2_PLACEMENT_3D('',#8373,#6304,#6305);
#5027=AXIS2_PLACEMENT_3D('',#8374,#6306,#6307);
#5028=AXIS2_PLACEMENT_3D('',#8398,#6313,#6314);
#5029=AXIS2_PLACEMENT_3D('',#8423,#6316,#6317);
#5030=AXIS2_PLACEMENT_3D('',#8443,#6321,#6322);
#5031=AXIS2_PLACEMENT_3D('',#8446,#6324,#6325);
#5032=AXIS2_PLACEMENT_3D('',#8448,#6327,#6328);
#5033=AXIS2_PLACEMENT_3D('',#8449,#6329,#6330);
#5034=AXIS2_PLACEMENT_3D('',#8451,#6331,#6332);
#5035=AXIS2_PLACEMENT_3D('',#8453,#6334,#6335);
#5036=AXIS2_PLACEMENT_3D('',#8454,#6336,#6337);
#5037=AXIS2_PLACEMENT_3D('',#8456,#6338,#6339);
#5038=AXIS2_PLACEMENT_3D('',#8458,#6340,#6341);
#5039=AXIS2_PLACEMENT_3D('',#8459,#6342,#6343);
#5040=AXIS2_PLACEMENT_3D('',#8466,#6345,#6346);
#5041=AXIS2_PLACEMENT_3D('',#8467,#6347,#6348);
#5042=AXIS2_PLACEMENT_3D('',#8495,#6349,#6350);
#5043=AXIS2_PLACEMENT_3D('',#8496,#6351,#6352);
#5044=AXIS2_PLACEMENT_3D('',#8497,#6353,#6354);
#5045=AXIS2_PLACEMENT_3D('',#8498,#6355,#6356);
#5046=AXIS2_PLACEMENT_3D('',#8500,#6358,#6359);
#5047=AXIS2_PLACEMENT_3D('',#8501,#6360,#6361);
#5048=AXIS2_PLACEMENT_3D('',#8502,#6362,#6363);
#5049=AXIS2_PLACEMENT_3D('',#8503,#6364,#6365);
#5050=AXIS2_PLACEMENT_3D('',#8504,#6366,#6367);
#5051=AXIS2_PLACEMENT_3D('',#8505,#6368,#6369);
#5052=AXIS2_PLACEMENT_3D('',#8506,#6370,#6371);
#5053=AXIS2_PLACEMENT_3D('',#8510,#6373,#6374);
#5054=AXIS2_PLACEMENT_3D('',#8514,#6376,#6377);
#5055=AXIS2_PLACEMENT_3D('',#8515,#6378,#6379);
#5056=AXIS2_PLACEMENT_3D('',#8518,#6381,#6382);
#5057=AXIS2_PLACEMENT_3D('',#8521,#6384,#6385);
#5058=AXIS2_PLACEMENT_3D('',#8522,#6386,#6387);
#5059=AXIS2_PLACEMENT_3D('',#8527,#6390,#6391);
#5060=AXIS2_PLACEMENT_3D('',#8530,#6394,#6395);
#5061=AXIS2_PLACEMENT_3D('',#8531,#6396,#6397);
#5062=AXIS2_PLACEMENT_3D('',#8532,#6398,#6399);
#5063=AXIS2_PLACEMENT_3D('',#8533,#6400,#6401);
#5064=DIRECTION('',(0.,0.,1.));
#5065=DIRECTION('',(1.,0.,0.));
#5066=DIRECTION('',(-0.866025403784439,0.5,0.));
#5067=DIRECTION('',(-0.5,-0.866025403784439,0.));
#5068=DIRECTION('',(0.,0.,-1.));
#5069=DIRECTION('',(0.,0.,-1.));
#5070=DIRECTION('',(0.5,0.866025403784439,0.));
#5071=DIRECTION('',(-0.866025403784438,-0.5,0.));
#5072=DIRECTION('',(0.5,-0.866025403784439,0.));
#5073=DIRECTION('',(0.,0.,-1.));
#5074=DIRECTION('',(-0.5,0.866025403784439,0.));
#5075=DIRECTION('',(0.,-1.,0.));
#5076=DIRECTION('',(0.,0.,-1.));
#5077=DIRECTION('',(0.,0.,-1.));
#5078=DIRECTION('',(-1.,0.,0.));
#5079=DIRECTION('',(0.866025403784439,-0.5,0.));
#5080=DIRECTION('',(0.5,0.866025403784439,0.));
#5081=DIRECTION('',(0.,0.,-1.));
#5082=DIRECTION('',(-0.5,-0.866025403784439,0.));
#5083=DIRECTION('',(0.866025403784438,0.5,0.));
#5084=DIRECTION('',(-0.5,0.866025403784438,0.));
#5085=DIRECTION('',(0.,0.,-1.));
#5086=DIRECTION('',(0.5,-0.866025403784439,0.));
#5087=DIRECTION('',(0.,1.,0.));
#5088=DIRECTION('',(0.,0.,1.));
#5089=DIRECTION('',(1.,0.,0.));
#5090=DIRECTION('',(0.,0.,1.));
#5091=DIRECTION('',(1.,0.,0.));
#5092=DIRECTION('',(0.,0.,1.));
#5093=DIRECTION('',(1.,0.,0.));
#5094=DIRECTION('',(0.,0.,1.));
#5095=DIRECTION('',(1.,0.,0.));
#5096=DIRECTION('',(0.,0.,-1.));
#5097=DIRECTION('',(-1.,0.,0.));
#5098=DIRECTION('',(0.,0.,1.));
#5099=DIRECTION('',(1.,0.,0.));
#5100=DIRECTION('',(0.,0.,-1.));
#5101=DIRECTION('',(1.,0.,0.));
#5102=DIRECTION('',(0.,0.,-1.));
#5103=DIRECTION('',(-1.,0.,0.));
#5104=DIRECTION('',(0.,0.,-1.));
#5105=DIRECTION('',(-1.,0.,0.));
#5106=DIRECTION('',(0.,0.,1.));
#5107=DIRECTION('',(1.,0.,0.));
#5108=DIRECTION('',(0.,0.,-1.));
#5109=DIRECTION('',(-1.,0.,0.));
#5110=DIRECTION('',(0.,0.,1.));
#5111=DIRECTION('',(1.,0.,0.));
#5112=DIRECTION('',(0.,0.,-1.));
#5113=DIRECTION('',(-1.,0.,0.));
#5114=DIRECTION('',(0.,0.,1.));
#5115=DIRECTION('',(1.,0.,0.));
#5116=DIRECTION('',(0.,0.,-1.));
#5117=DIRECTION('',(-1.,0.,0.));
#5118=DIRECTION('',(0.,0.,1.));
#5119=DIRECTION('',(1.,0.,0.));
#5120=DIRECTION('',(0.,0.,-1.));
#5121=DIRECTION('',(-1.,0.,0.));
#5122=DIRECTION('',(0.,0.,1.));
#5123=DIRECTION('',(1.,0.,0.));
#5124=DIRECTION('',(0.,0.,-1.));
#5125=DIRECTION('',(-1.,0.,0.));
#5126=DIRECTION('',(0.,0.,1.));
#5127=DIRECTION('',(1.,0.,0.));
#5128=DIRECTION('',(0.,0.,1.));
#5129=DIRECTION('',(1.,0.,0.));
#5130=DIRECTION('',(0.,0.,1.));
#5131=DIRECTION('',(1.,0.,0.));
#5132=DIRECTION('',(0.,0.,1.));
#5133=DIRECTION('',(1.,0.,0.));
#5134=DIRECTION('',(1.26117795448129E-16,-2.49800180540662E-16,-1.));
#5135=DIRECTION('',(6.93889390390706E-18,-1.,2.49800180540662E-16));
#5136=DIRECTION('',(0.,1.,0.));
#5137=DIRECTION('',(0.,0.,1.));
#5138=DIRECTION('',(0.,1.,0.));
#5139=DIRECTION('',(1.,0.,0.));
#5140=DIRECTION('',(0.,1.,0.));
#5141=DIRECTION('',(0.,0.,1.));
#5142=DIRECTION('',(0.,1.,0.));
#5143=DIRECTION('',(0.,0.,1.));
#5144=DIRECTION('',(0.,1.,0.));
#5145=DIRECTION('',(1.,0.,0.));
#5146=DIRECTION('',(0.,1.,0.));
#5147=DIRECTION('',(0.,0.,1.));
#5148=DIRECTION('',(0.,-1.,0.));
#5149=DIRECTION('',(0.,0.,-1.));
#5150=DIRECTION('',(0.,-1.,0.));
#5151=DIRECTION('',(0.,0.,-1.));
#5152=DIRECTION('',(0.,-1.,-4.5102810375397E-16));
#5153=DIRECTION('',(1.,0.,0.));
#5154=DIRECTION('',(0.,-1.,0.));
#5155=DIRECTION('',(0.,0.,-1.));
#5156=DIRECTION('',(0.,1.,0.));
#5157=DIRECTION('',(0.,0.,1.));
#5158=DIRECTION('',(0.,-1.,0.));
#5159=DIRECTION('',(0.,1.,0.));
#5160=DIRECTION('',(0.,0.,1.));
#5161=DIRECTION('',(0.,-1.,0.));
#5162=DIRECTION('',(1.,0.,2.45338361172824E-16));
#5163=DIRECTION('',(2.45338361172824E-16,0.,-1.));
#5164=DIRECTION('',(-2.45338361172824E-16,0.,1.));
#5165=DIRECTION('',(0.,-1.,0.));
#5166=DIRECTION('',(-2.45338361172824E-16,0.,1.));
#5167=DIRECTION('',(0.,-1.,0.));
#5168=DIRECTION('',(0.,0.,-1.));
#5169=DIRECTION('',(0.,-1.,0.));
#5170=DIRECTION('',(0.,0.,1.));
#5171=DIRECTION('',(0.,-1.,0.));
#5172=DIRECTION('',(0.,-1.,0.));
#5173=DIRECTION('',(0.,0.,1.));
#5174=DIRECTION('',(-1.,0.,-2.45338361172824E-16));
#5175=DIRECTION('',(-2.45338361172824E-16,0.,1.));
#5176=DIRECTION('',(2.45338361172824E-16,0.,-1.));
#5177=DIRECTION('',(2.45338361172824E-16,0.,-1.));
#5178=DIRECTION('',(0.,1.,0.));
#5179=DIRECTION('',(0.,0.,1.));
#5180=DIRECTION('',(0.,1.,0.));
#5181=DIRECTION('',(0.,0.,1.));
#5182=DIRECTION('',(-1.,-2.22044604925032E-16,1.21685779376401E-16));
#5183=DIRECTION('',(-2.22044604925032E-16,1.,4.570614031279E-16));
#5184=DIRECTION('',(0.,0.,1.));
#5185=DIRECTION('',(1.,0.,0.));
#5186=DIRECTION('',(0.,0.,1.));
#5187=DIRECTION('',(1.,0.,0.));
#5188=DIRECTION('',(1.82918119333769E-16,-1.,0.));
#5189=DIRECTION('',(1.,1.82918119333769E-16,0.));
#5190=DIRECTION('',(1.82918119333769E-16,-1.,0.));
#5191=DIRECTION('',(1.,1.82918119333769E-16,0.));
#5192=DIRECTION('',(1.82918119333769E-16,-1.,0.));
#5193=DIRECTION('',(1.,1.82918119333769E-16,0.));
#5194=DIRECTION('',(1.82918119333769E-16,-1.,0.));
#5195=DIRECTION('',(1.,1.82918119333769E-16,0.));
#5196=DIRECTION('',(1.82918119333769E-16,-1.,0.));
#5197=DIRECTION('',(1.,1.82918119333769E-16,0.));
#5198=DIRECTION('',(1.82918119333769E-16,-1.,0.));
#5199=DIRECTION('',(1.,1.82918119333769E-16,0.));
#5200=DIRECTION('',(-1.82918119333769E-16,1.,0.));
#5201=DIRECTION('',(-1.,-1.82918119333769E-16,0.));
#5202=DIRECTION('',(1.82918119333769E-16,-1.,0.));
#5203=DIRECTION('',(1.,1.82918119333769E-16,0.));
#5204=DIRECTION('',(1.82918119333769E-16,-1.,0.));
#5205=DIRECTION('',(1.,1.82918119333769E-16,0.));
#5206=DIRECTION('',(1.82918119333769E-16,-1.,0.));
#5207=DIRECTION('',(1.,1.82918119333769E-16,0.));
#5208=DIRECTION('',(1.82918119333769E-16,-1.,0.));
#5209=DIRECTION('',(1.,1.82918119333769E-16,0.));
#5210=DIRECTION('',(1.82918119333769E-16,-1.,0.));
#5211=DIRECTION('',(1.,1.82918119333769E-16,0.));
#5212=DIRECTION('',(1.82918119333769E-16,-1.,0.));
#5213=DIRECTION('',(1.,1.82918119333769E-16,0.));
#5214=DIRECTION('',(1.82918119333769E-16,-1.,0.));
#5215=DIRECTION('',(1.,1.82918119333769E-16,0.));
#5216=DIRECTION('',(-1.82918119333769E-16,1.,0.));
#5217=DIRECTION('',(-1.,-1.82918119333769E-16,0.));
#5218=DIRECTION('',(1.82918119333769E-16,-1.,0.));
#5219=DIRECTION('',(1.,1.82918119333769E-16,0.));
#5220=DIRECTION('',(1.82918119333769E-16,-1.,0.));
#5221=DIRECTION('',(1.,1.82918119333769E-16,0.));
#5222=DIRECTION('',(1.82918119333769E-16,-1.,0.));
#5223=DIRECTION('',(1.,1.82918119333769E-16,0.));
#5224=DIRECTION('',(1.82918119333769E-16,-1.,0.));
#5225=DIRECTION('',(1.,1.82918119333769E-16,0.));
#5226=DIRECTION('',(1.82918119333769E-16,-1.,0.));
#5227=DIRECTION('',(1.,1.82918119333769E-16,0.));
#5228=DIRECTION('',(1.82918119333769E-16,-1.,0.));
#5229=DIRECTION('',(1.,1.82918119333769E-16,0.));
#5230=DIRECTION('',(1.82918119333769E-16,-1.,0.));
#5231=DIRECTION('',(1.,1.82918119333769E-16,0.));
#5232=DIRECTION('',(-1.82918119333769E-16,1.,0.));
#5233=DIRECTION('',(-1.,-1.82918119333769E-16,0.));
#5234=DIRECTION('',(1.82918119333769E-16,-1.,0.));
#5235=DIRECTION('',(1.,1.82918119333769E-16,0.));
#5236=DIRECTION('',(1.82918119333769E-16,-1.,0.));
#5237=DIRECTION('',(1.,1.82918119333769E-16,0.));
#5238=DIRECTION('',(1.82918119333769E-16,-1.,0.));
#5239=DIRECTION('',(1.,1.82918119333769E-16,0.));
#5240=DIRECTION('',(1.82918119333769E-16,-1.,0.));
#5241=DIRECTION('',(1.,1.82918119333769E-16,0.));
#5242=DIRECTION('',(1.82918119333769E-16,-1.,0.));
#5243=DIRECTION('',(1.,1.82918119333769E-16,0.));
#5244=DIRECTION('',(1.82918119333769E-16,-1.,0.));
#5245=DIRECTION('',(1.,1.82918119333769E-16,0.));
#5246=DIRECTION('',(1.82918119333769E-16,-1.,0.));
#5247=DIRECTION('',(1.,1.82918119333769E-16,0.));
#5248=DIRECTION('',(-1.82918119333769E-16,1.,0.));
#5249=DIRECTION('',(-1.,-1.82918119333769E-16,0.));
#5250=DIRECTION('',(1.82918119333769E-16,-1.,0.));
#5251=DIRECTION('',(1.,1.82918119333769E-16,0.));
#5252=DIRECTION('',(1.82918119333769E-16,-1.,0.));
#5253=DIRECTION('',(1.,1.82918119333769E-16,0.));
#5254=DIRECTION('',(1.82918119333769E-16,-1.,0.));
#5255=DIRECTION('',(1.,1.82918119333769E-16,0.));
#5256=DIRECTION('',(1.82918119333769E-16,-1.,0.));
#5257=DIRECTION('',(1.,1.82918119333769E-16,0.));
#5258=DIRECTION('',(1.82918119333769E-16,-1.,0.));
#5259=DIRECTION('',(1.,1.82918119333769E-16,0.));
#5260=DIRECTION('',(1.82918119333769E-16,-1.,0.));
#5261=DIRECTION('',(1.,1.82918119333769E-16,0.));
#5262=DIRECTION('',(1.82918119333769E-16,-1.,0.));
#5263=DIRECTION('',(1.,1.82918119333769E-16,0.));
#5264=DIRECTION('',(-1.82918119333769E-16,1.,0.));
#5265=DIRECTION('',(-1.,-1.82918119333769E-16,0.));
#5266=DIRECTION('',(1.82918119333769E-16,-1.,0.));
#5267=DIRECTION('',(1.,1.82918119333769E-16,0.));
#5268=DIRECTION('',(1.82918119333769E-16,-1.,0.));
#5269=DIRECTION('',(1.,1.82918119333769E-16,0.));
#5270=DIRECTION('',(0.,0.,-1.));
#5271=DIRECTION('',(-1.,0.,0.));
#5272=DIRECTION('',(0.,0.,1.));
#5273=DIRECTION('',(1.,0.,0.));
#5274=DIRECTION('',(0.,0.,1.));
#5275=DIRECTION('',(1.,0.,0.));
#5276=DIRECTION('',(0.,0.,1.));
#5277=DIRECTION('',(-1.,0.,0.));
#5278=DIRECTION('',(0.,0.,1.));
#5279=DIRECTION('',(1.,0.,0.));
#5280=DIRECTION('',(0.,0.,-1.));
#5281=DIRECTION('',(1.,0.,0.));
#5282=DIRECTION('',(0.,0.,1.));
#5283=DIRECTION('',(1.,0.,0.));
#5284=DIRECTION('',(0.,0.,1.));
#5285=DIRECTION('',(1.,0.,0.));
#5286=DIRECTION('',(-1.,-2.42861286636753E-16,1.21685779376401E-16));
#5287=DIRECTION('',(2.42861286636753E-16,-1.,-6.39979522461685E-16));
#5288=DIRECTION('',(1.,3.46944695195361E-17,6.12323399573681E-17));
#5289=DIRECTION('',(3.46944695195361E-17,-1.,-4.51028103753972E-16));
#5290=DIRECTION('',(-1.216857793764E-16,-6.39953377497951E-16,-1.));
#5291=DIRECTION('',(1.80411241501588E-16,-1.,6.39953377497951E-16));
#5292=DIRECTION('',(0.,0.,1.));
#5293=DIRECTION('',(1.,0.,0.));
#5294=DIRECTION('',(0.,0.,1.));
#5295=DIRECTION('',(1.,0.,0.));
#5296=DIRECTION('',(0.,0.,1.));
#5297=DIRECTION('',(1.,0.,0.));
#5298=DIRECTION('',(0.,0.,1.));
#5299=DIRECTION('',(1.,0.,0.));
#5300=DIRECTION('',(0.,0.,1.));
#5301=DIRECTION('',(1.,0.,0.));
#5302=DIRECTION('',(0.,0.,1.));
#5303=DIRECTION('',(1.,0.,0.));
#5304=DIRECTION('',(0.,0.,-1.));
#5305=DIRECTION('',(-1.,0.,0.));
#5306=DIRECTION('',(0.,0.,1.));
#5307=DIRECTION('',(1.,0.,0.));
#5308=DIRECTION('',(-1.,-2.56739074444568E-16,1.21685779376401E-16));
#5309=DIRECTION('',(2.56739074444567E-16,-1.,-5.12260443711339E-16));
#5310=DIRECTION('',(0.,0.,1.));
#5311=DIRECTION('',(1.,0.,0.));
#5312=DIRECTION('',(0.,0.,1.));
#5313=DIRECTION('',(0.,1.11917643611407E-16,-1.));
#5314=DIRECTION('',(0.,1.,1.11917643611407E-16));
#5315=DIRECTION('',(0.,0.,1.));
#5316=DIRECTION('',(0.,1.11917643611407E-16,-1.));
#5317=DIRECTION('',(0.,1.,1.11917643611407E-16));
#5318=DIRECTION('',(0.,1.11917643611407E-16,-1.));
#5319=DIRECTION('',(0.,1.,1.11917643611407E-16));
#5320=DIRECTION('',(0.,1.11917643611407E-16,-1.));
#5321=DIRECTION('',(0.,1.,1.11917643611407E-16));
#5322=DIRECTION('',(0.,1.11917643611407E-16,-1.));
#5323=DIRECTION('',(0.,1.,1.11917643611407E-16));
#5324=DIRECTION('',(0.,1.11917643611407E-16,-1.));
#5325=DIRECTION('',(0.,1.,1.11917643611407E-16));
#5326=DIRECTION('',(-1.,-3.90153196957302E-16,-4.36650264509183E-32));
#5327=DIRECTION('',(3.90153196957302E-16,-1.,0.));
#5328=DIRECTION('',(0.707106781186548,-0.707106781186548,-7.91377247320451E-17));
#5329=DIRECTION('',(-0.707106781186548,-0.707106781186548,-7.91377247320451E-17));
#5330=DIRECTION('',(1.,3.90153196957302E-16,4.36650264509183E-32));
#5331=DIRECTION('',(1.,3.90153196957302E-16,4.36650264509183E-32));
#5332=DIRECTION('',(-1.,-3.90153196957302E-16,-4.36650264509183E-32));
#5333=DIRECTION('',(3.90153196957302E-16,-1.,0.));
#5334=DIRECTION('',(-0.707106781186548,0.707106781186548,7.91377247320451E-17));
#5335=DIRECTION('',(0.707106781186548,0.707106781186548,7.91377247320451E-17));
#5336=DIRECTION('',(-1.,-3.90153196957302E-16,-4.36650264509183E-32));
#5337=DIRECTION('',(-1.,-3.90153196957302E-16,-4.36650264509183E-32));
#5338=DIRECTION('',(-1.,0.,0.));
#5339=DIRECTION('',(0.,0.,1.));
#5340=DIRECTION('',(1.,0.,0.));
#5341=DIRECTION('',(0.707106781186548,0.707106781186548,7.91377247320451E-17));
#5342=DIRECTION('',(-0.707106781186548,0.707106781186548,7.91377247320451E-17));
#5343=DIRECTION('',(1.,0.,0.));
#5344=DIRECTION('',(-1.,0.,0.));
#5345=DIRECTION('',(0.,0.,1.));
#5346=DIRECTION('',(-1.,0.,0.));
#5347=DIRECTION('',(-0.707106781186548,-0.707106781186548,-7.91377247320451E-17));
#5348=DIRECTION('',(0.707106781186548,-0.707106781186548,-7.91377247320451E-17));
#5349=DIRECTION('',(-1.,0.,0.));
#5350=DIRECTION('',(0.,1.,1.11917643611407E-16));
#5351=DIRECTION('',(0.,-1.11917643611407E-16,1.));
#5352=DIRECTION('',(0.,-1.,0.));
#5353=DIRECTION('',(0.,0.,-1.));
#5354=DIRECTION('',(0.,-1.,-1.11917643611407E-16));
#5355=DIRECTION('',(0.,-1.,-1.11917643611407E-16));
#5356=DIRECTION('',(0.,-1.,-1.11917643611407E-16));
#5357=DIRECTION('',(0.,1.11917643611407E-16,-1.));
#5358=DIRECTION('',(0.,-1.,0.));
#5359=DIRECTION('',(0.,0.,-1.));
#5360=DIRECTION('',(0.,-1.,-1.11917643611407E-16));
#5361=DIRECTION('',(0.,-1.,-1.11917643611407E-16));
#5362=DIRECTION('',(-1.,0.,0.));
#5363=DIRECTION('',(0.,0.,1.));
#5364=DIRECTION('',(0.,0.,1.));
#5365=DIRECTION('',(0.,0.,-1.));
#5366=DIRECTION('',(0.,0.,-1.));
#5367=DIRECTION('',(1.,0.,0.));
#5368=DIRECTION('',(-1.,0.,0.));
#5369=DIRECTION('',(0.,0.,1.));
#5370=DIRECTION('',(1.,0.,0.));
#5371=DIRECTION('',(-1.,0.,0.));
#5372=DIRECTION('',(0.,0.,1.));
#5373=DIRECTION('',(1.,0.,0.));
#5374=DIRECTION('',(0.,1.11917643611407E-16,-1.));
#5375=DIRECTION('',(0.,1.,1.11917643611407E-16));
#5376=DIRECTION('',(0.,1.11917643611407E-16,-1.));
#5377=DIRECTION('',(0.,1.,1.11917643611407E-16));
#5378=DIRECTION('',(0.,1.11917643611407E-16,-1.));
#5379=DIRECTION('',(0.,1.,1.11917643611407E-16));
#5380=DIRECTION('',(0.,0.,1.));
#5381=DIRECTION('',(1.,0.,0.));
#5382=DIRECTION('',(0.,0.,1.));
#5383=DIRECTION('',(0.,0.,1.));
#5384=DIRECTION('',(0.,1.11917643611407E-16,-1.));
#5385=DIRECTION('',(0.,1.,1.11917643611407E-16));
#5386=DIRECTION('',(0.,1.11917643611407E-16,-1.));
#5387=DIRECTION('',(0.,1.,1.11917643611407E-16));
#5388=DIRECTION('',(0.,1.11917643611407E-16,-1.));
#5389=DIRECTION('',(0.,1.,1.11917643611407E-16));
#5390=DIRECTION('',(0.,0.,1.));
#5391=DIRECTION('',(1.,0.,0.));
#5392=DIRECTION('',(1.,0.,0.));
#5393=DIRECTION('',(0.,0.,1.));
#5394=DIRECTION('',(1.,0.,0.));
#5395=DIRECTION('',(1.,0.,0.));
#5396=DIRECTION('',(0.,0.,1.));
#5397=DIRECTION('',(1.,0.,0.));
#5398=DIRECTION('',(0.,0.,-1.));
#5399=DIRECTION('',(-1.,0.,0.));
#5400=DIRECTION('',(0.,0.,-1.));
#5401=DIRECTION('',(0.,0.,-1.));
#5402=DIRECTION('',(0.,0.,1.));
#5403=DIRECTION('',(1.,0.,0.));
#5404=DIRECTION('',(0.,0.,1.));
#5405=DIRECTION('',(0.,0.,1.));
#5406=DIRECTION('',(0.,-1.,-1.11917643611407E-16));
#5407=DIRECTION('',(0.,1.11917643611407E-16,-1.));
#5408=DIRECTION('',(0.,-1.,0.));
#5409=DIRECTION('',(0.,0.,-1.));
#5410=DIRECTION('',(0.,-1.,-1.11917643611407E-16));
#5411=DIRECTION('',(0.,-1.,-1.11917643611407E-16));
#5412=DIRECTION('',(0.,1.,1.11917643611407E-16));
#5413=DIRECTION('',(0.,-1.11917643611407E-16,1.));
#5414=DIRECTION('',(0.,-1.,0.));
#5415=DIRECTION('',(0.,0.,-1.));
#5416=DIRECTION('',(0.,-1.,-1.11917643611407E-16));
#5417=DIRECTION('',(0.,-1.,-1.11917643611407E-16));
#5418=DIRECTION('',(-1.,0.,0.));
#5419=DIRECTION('',(0.,0.,1.));
#5420=DIRECTION('',(0.,0.,1.));
#5421=DIRECTION('',(0.,0.,-1.));
#5422=DIRECTION('',(0.,1.11917643611407E-16,-1.));
#5423=DIRECTION('',(0.,1.,1.11917643611407E-16));
#5424=DIRECTION('',(-1.,0.,0.));
#5425=DIRECTION('',(-1.,0.,0.));
#5426=DIRECTION('',(0.,1.11917643611407E-16,-1.));
#5427=DIRECTION('',(0.,1.,1.11917643611407E-16));
#5428=DIRECTION('',(-1.,0.,0.));
#5429=DIRECTION('',(-1.,0.,0.));
#5430=DIRECTION('',(-3.90153196957302E-16,1.,0.));
#5431=DIRECTION('',(-1.,-3.90153196957302E-16,0.));
#5432=DIRECTION('',(-3.90153196957302E-16,1.,0.));
#5433=DIRECTION('',(-1.,-3.90153196957302E-16,0.));
#5434=DIRECTION('',(0.,1.,0.));
#5435=DIRECTION('',(0.,0.,1.));
#5436=DIRECTION('',(0.,-1.,0.));
#5437=DIRECTION('',(0.,0.,-1.));
#5438=DIRECTION('',(0.,1.,0.));
#5439=DIRECTION('',(0.,0.,1.));
#5440=DIRECTION('',(0.,1.,0.));
#5441=DIRECTION('',(0.,0.,1.));
#5442=DIRECTION('',(0.,1.,0.));
#5443=DIRECTION('',(0.,0.,1.));
#5444=DIRECTION('',(0.,-1.,0.));
#5445=DIRECTION('',(0.,0.,-1.));
#5446=DIRECTION('',(0.,-1.,0.));
#5447=DIRECTION('',(1.,0.,0.));
#5448=DIRECTION('',(0.,-1.,0.));
#5449=DIRECTION('',(1.,0.,0.));
#5450=DIRECTION('',(-1.,-1.80411241501588E-16,1.21685779376401E-16));
#5451=DIRECTION('',(1.80411241501588E-16,-1.,2.4980018054066E-16));
#5452=DIRECTION('',(-1.38777878078145E-16,1.,4.57061403127902E-16));
#5453=DIRECTION('',(1.,1.38777878078145E-16,-1.21685779376413E-16));
#5454=DIRECTION('',(0.,1.11917643611407E-16,-1.));
#5455=DIRECTION('',(0.,1.,1.11917643611407E-16));
#5456=DIRECTION('',(0.,-1.,-1.11917643611407E-16));
#5457=DIRECTION('',(-1.,0.,0.));
#5458=DIRECTION('',(0.,1.11917643611407E-16,-1.));
#5459=DIRECTION('',(0.,1.,1.11917643611407E-16));
#5460=DIRECTION('',(-1.,0.,0.));
#5461=DIRECTION('',(0.,-1.,-1.11917643611407E-16));
#5462=DIRECTION('',(0.,1.11917643611407E-16,-1.));
#5463=DIRECTION('',(0.,1.,1.11917643611407E-16));
#5464=DIRECTION('',(0.,1.11917643611407E-16,-1.));
#5465=DIRECTION('',(0.,1.,1.11917643611407E-16));
#5466=DIRECTION('',(0.,1.11917643611407E-16,-1.));
#5467=DIRECTION('',(0.,1.,1.11917643611407E-16));
#5468=DIRECTION('',(0.,1.11917643611407E-16,-1.));
#5469=DIRECTION('',(0.,1.,1.11917643611407E-16));
#5470=DIRECTION('',(-1.,0.,0.));
#5471=DIRECTION('',(0.,-1.,-1.11917643611407E-16));
#5472=DIRECTION('',(0.,1.11917643611407E-16,-1.));
#5473=DIRECTION('',(0.,1.,1.11917643611407E-16));
#5474=DIRECTION('',(0.,1.11917643611407E-16,-1.));
#5475=DIRECTION('',(0.,1.,1.11917643611407E-16));
#5476=DIRECTION('',(0.,1.11917643611407E-16,-1.));
#5477=DIRECTION('',(0.,1.,1.11917643611407E-16));
#5478=DIRECTION('',(0.,-1.,-1.11917643611407E-16));
#5479=DIRECTION('',(-1.,0.,0.));
#5480=DIRECTION('',(0.,1.11917643611407E-16,-1.));
#5481=DIRECTION('',(0.,1.,1.11917643611407E-16));
#5482=DIRECTION('',(-1.,0.,0.));
#5483=DIRECTION('',(0.,0.,1.));
#5484=DIRECTION('',(0.,0.,1.));
#5485=DIRECTION('',(0.,-1.,-1.11917643611407E-16));
#5486=DIRECTION('',(0.,0.,-1.));
#5487=DIRECTION('',(0.,-1.,-1.11917643611407E-16));
#5488=DIRECTION('',(-1.,0.,0.));
#5489=DIRECTION('',(0.,0.,1.));
#5490=DIRECTION('',(0.,-1.,-1.11917643611407E-16));
#5491=DIRECTION('',(0.,0.,1.));
#5492=DIRECTION('',(0.,-1.,-1.11917643611407E-16));
#5493=DIRECTION('',(0.,0.,-1.));
#5494=DIRECTION('',(0.,0.,1.));
#5495=DIRECTION('',(1.,0.,0.));
#5496=DIRECTION('',(0.,0.,1.));
#5497=DIRECTION('',(0.,0.,1.));
#5498=DIRECTION('',(1.,0.,0.));
#5499=DIRECTION('',(0.,0.,1.));
#5500=DIRECTION('',(0.,0.,1.));
#5501=DIRECTION('',(1.,0.,0.));
#5502=DIRECTION('',(0.,1.,0.));
#5503=DIRECTION('',(0.,0.,1.));
#5504=DIRECTION('',(0.,-1.,0.));
#5505=DIRECTION('',(0.,0.,-1.));
#5506=DIRECTION('',(0.,1.,0.));
#5507=DIRECTION('',(0.,0.,1.));
#5508=DIRECTION('',(0.,-1.,0.));
#5509=DIRECTION('',(0.,0.,-1.));
#5510=DIRECTION('',(0.,0.,-1.));
#5511=DIRECTION('',(-1.,0.,0.));
#5512=DIRECTION('',(0.,0.,-1.));
#5513=DIRECTION('',(0.,0.,1.));
#5514=DIRECTION('',(1.,0.,0.));
#5515=DIRECTION('',(0.,0.,-1.));
#5516=DIRECTION('',(0.,1.11917643611407E-16,-1.));
#5517=DIRECTION('',(0.,1.,1.11917643611407E-16));
#5518=DIRECTION('',(0.,0.,1.));
#5519=DIRECTION('',(1.,0.,0.));
#5520=DIRECTION('',(1.,0.,0.));
#5521=DIRECTION('',(1.,0.,0.));
#5522=DIRECTION('',(0.,0.,1.));
#5523=DIRECTION('',(1.,0.,0.));
#5524=DIRECTION('',(0.,1.11917643611407E-16,-1.));
#5525=DIRECTION('',(0.,1.,1.11917643611407E-16));
#5526=DIRECTION('',(0.,0.,1.));
#5527=DIRECTION('',(0.,0.,1.));
#5528=DIRECTION('',(1.,0.,0.));
#5529=DIRECTION('',(0.,0.,1.));
#5530=DIRECTION('',(0.,0.,-1.));
#5531=DIRECTION('',(1.,0.,0.));
#5532=DIRECTION('',(-1.,0.,0.));
#5533=DIRECTION('',(-1.,0.,0.));
#5534=DIRECTION('',(0.,-1.,-1.11917643611407E-16));
#5535=DIRECTION('',(0.,1.11917643611407E-16,-1.));
#5536=DIRECTION('',(0.,-1.,0.));
#5537=DIRECTION('',(0.,0.,-1.));
#5538=DIRECTION('',(0.,-1.,0.));
#5539=DIRECTION('',(0.,0.,-1.));
#5540=DIRECTION('',(0.,1.,1.11917643611407E-16));
#5541=DIRECTION('',(0.,-1.11917643611407E-16,1.));
#5542=DIRECTION('',(0.,-1.,0.));
#5543=DIRECTION('',(0.,0.,-1.));
#5544=DIRECTION('',(0.,-1.,0.));
#5545=DIRECTION('',(0.,0.,-1.));
#5546=DIRECTION('',(0.,1.,1.11917643611407E-16));
#5547=DIRECTION('',(0.,-1.11917643611407E-16,1.));
#5548=DIRECTION('',(0.,-1.,0.));
#5549=DIRECTION('',(0.,0.,-1.));
#5550=DIRECTION('',(0.,1.,0.));
#5551=DIRECTION('',(0.,0.,1.));
#5552=DIRECTION('',(0.,-1.,-1.11917643611407E-16));
#5553=DIRECTION('',(0.,1.11917643611407E-16,-1.));
#5554=DIRECTION('',(0.,-1.,0.));
#5555=DIRECTION('',(0.,0.,-1.));
#5556=DIRECTION('',(0.,1.,0.));
#5557=DIRECTION('',(0.,0.,1.));
#5558=DIRECTION('',(0.,1.11917643611407E-16,-1.));
#5559=DIRECTION('',(0.,1.,1.11917643611407E-16));
#5560=DIRECTION('',(0.,1.11917643611407E-16,-1.));
#5561=DIRECTION('',(0.,1.,1.11917643611407E-16));
#5562=DIRECTION('',(0.,7.65524871482112E-17,-1.));
#5563=DIRECTION('',(0.,1.,7.65524871482112E-17));
#5564=DIRECTION('',(-0.0560813448397478,-0.998426202961924,-7.643200907068E-17));
#5565=DIRECTION('',(0.,7.65524871482112E-17,-1.));
#5566=DIRECTION('',(0.,1.,7.65524871482112E-17));
#5567=DIRECTION('',(0.,7.65524871482112E-17,-1.));
#5568=DIRECTION('',(0.,1.,7.65524871482112E-17));
#5569=DIRECTION('',(0.,7.65524871482112E-17,-1.));
#5570=DIRECTION('',(0.,1.,7.65524871482112E-17));
#5571=DIRECTION('',(0.0560813448397477,0.998426202961924,7.643200907068E-17));
#5572=DIRECTION('',(0.,7.65524871482112E-17,-1.));
#5573=DIRECTION('',(0.,1.,7.65524871482112E-17));
#5574=DIRECTION('',(0.,7.65524871482112E-17,-1.));
#5575=DIRECTION('',(0.,1.,7.65524871482112E-17));
#5576=DIRECTION('',(0.,7.65524871482112E-17,-1.));
#5577=DIRECTION('',(0.,1.,7.65524871482112E-17));
#5578=DIRECTION('',(0.,1.14828730722317E-16,-1.));
#5579=DIRECTION('',(0.,1.,1.14828730722317E-16));
#5580=DIRECTION('',(0.0560813448397478,-0.998426202961924,-1.1464801360602E-16));
#5581=DIRECTION('',(0.,1.14828730722317E-16,-1.));
#5582=DIRECTION('',(0.,1.,1.14828730722317E-16));
#5583=DIRECTION('',(0.,1.14828730722317E-16,-1.));
#5584=DIRECTION('',(0.,1.,1.14828730722317E-16));
#5585=DIRECTION('',(0.,1.14828730722317E-16,-1.));
#5586=DIRECTION('',(0.,1.,1.14828730722317E-16));
#5587=DIRECTION('',(-0.0560813448397477,0.998426202961924,1.1464801360602E-16));
#5588=DIRECTION('',(0.,1.14828730722317E-16,-1.));
#5589=DIRECTION('',(0.,1.,1.14828730722317E-16));
#5590=DIRECTION('',(0.,1.14828730722317E-16,-1.));
#5591=DIRECTION('',(0.,1.,1.14828730722317E-16));
#5592=DIRECTION('',(0.,1.14828730722317E-16,-1.));
#5593=DIRECTION('',(0.,1.,1.14828730722317E-16));
#5594=DIRECTION('',(0.,0.,-1.));
#5595=DIRECTION('',(-1.,0.,0.));
#5596=DIRECTION('',(0.,0.,-1.));
#5597=DIRECTION('',(-1.,0.,0.));
#5598=DIRECTION('',(0.,0.,-1.));
#5599=DIRECTION('',(-1.,0.,0.));
#5600=DIRECTION('',(-1.,0.,0.));
#5601=DIRECTION('',(0.,0.,-1.));
#5602=DIRECTION('',(-1.,0.,0.));
#5603=DIRECTION('',(0.,0.,-1.));
#5604=DIRECTION('',(-1.,0.,0.));
#5605=DIRECTION('',(0.,0.,-1.));
#5606=DIRECTION('',(-1.,0.,0.));
#5607=DIRECTION('',(0.,0.,-1.));
#5608=DIRECTION('',(-1.,0.,0.));
#5609=DIRECTION('',(0.,0.,1.));
#5610=DIRECTION('',(1.,0.,0.));
#5611=DIRECTION('',(0.,0.,1.));
#5612=DIRECTION('',(0.,0.,-1.));
#5613=DIRECTION('',(-1.,0.,0.));
#5614=DIRECTION('',(0.,1.14828730722317E-16,-1.));
#5615=DIRECTION('',(0.,1.,1.14828730722317E-16));
#5616=DIRECTION('',(0.,0.,1.));
#5617=DIRECTION('',(0.,7.65524871482112E-17,-1.));
#5618=DIRECTION('',(0.,1.,7.65524871482112E-17));
#5619=DIRECTION('',(0.,0.,-1.));
#5620=DIRECTION('',(-1.,0.,0.));
#5621=DIRECTION('',(0.,0.,1.));
#5622=DIRECTION('',(1.,0.,0.));
#5623=DIRECTION('',(0.,0.,-1.));
#5624=DIRECTION('',(-1.,0.,0.));
#5625=DIRECTION('',(0.,0.,1.));
#5626=DIRECTION('',(0.,0.,-1.));
#5627=DIRECTION('',(-1.,0.,0.));
#5628=DIRECTION('',(0.,7.65524871482112E-17,-1.));
#5629=DIRECTION('',(0.,1.,7.65524871482112E-17));
#5630=DIRECTION('',(0.,0.,1.));
#5631=DIRECTION('',(0.,1.14828730722317E-16,-1.));
#5632=DIRECTION('',(0.,1.,1.14828730722317E-16));
#5633=DIRECTION('',(0.,0.,-1.));
#5634=DIRECTION('',(-1.,0.,0.));
#5635=DIRECTION('',(0.,0.,-1.));
#5636=DIRECTION('',(-1.,0.,0.));
#5637=DIRECTION('',(0.,0.,-1.));
#5638=DIRECTION('',(-1.,0.,0.));
#5639=DIRECTION('',(-1.,0.,0.));
#5640=DIRECTION('',(0.,0.,-1.));
#5641=DIRECTION('',(-1.,0.,0.));
#5642=DIRECTION('',(0.,0.,-1.));
#5643=DIRECTION('',(-1.,0.,0.));
#5644=DIRECTION('',(0.,0.,-1.));
#5645=DIRECTION('',(-1.,0.,0.));
#5646=DIRECTION('',(0.,0.,-1.));
#5647=DIRECTION('',(-1.,0.,0.));
#5648=DIRECTION('',(0.,7.65524871482112E-17,-1.));
#5649=DIRECTION('',(0.,1.,7.65524871482112E-17));
#5650=DIRECTION('',(0.0560813448397478,-0.998426202961924,-7.643200907068E-17));
#5651=DIRECTION('',(0.,7.65524871482112E-17,-1.));
#5652=DIRECTION('',(0.,1.,7.65524871482112E-17));
#5653=DIRECTION('',(0.,7.65524871482112E-17,-1.));
#5654=DIRECTION('',(0.,1.,7.65524871482112E-17));
#5655=DIRECTION('',(0.,7.65524871482112E-17,-1.));
#5656=DIRECTION('',(0.,1.,7.65524871482112E-17));
#5657=DIRECTION('',(-0.0560813448397477,0.998426202961924,7.643200907068E-17));
#5658=DIRECTION('',(0.,7.65524871482112E-17,-1.));
#5659=DIRECTION('',(0.,1.,7.65524871482112E-17));
#5660=DIRECTION('',(0.,7.65524871482112E-17,-1.));
#5661=DIRECTION('',(0.,1.,7.65524871482112E-17));
#5662=DIRECTION('',(0.,7.65524871482112E-17,-1.));
#5663=DIRECTION('',(0.,1.,7.65524871482112E-17));
#5664=DIRECTION('',(0.,1.14828730722317E-16,-1.));
#5665=DIRECTION('',(0.,1.,1.14828730722317E-16));
#5666=DIRECTION('',(-0.0560813448397478,-0.998426202961924,-1.1464801360602E-16));
#5667=DIRECTION('',(0.,1.14828730722317E-16,-1.));
#5668=DIRECTION('',(0.,1.,1.14828730722317E-16));
#5669=DIRECTION('',(0.,1.14828730722317E-16,-1.));
#5670=DIRECTION('',(0.,1.,1.14828730722317E-16));
#5671=DIRECTION('',(0.,1.14828730722317E-16,-1.));
#5672=DIRECTION('',(0.,1.,1.14828730722317E-16));
#5673=DIRECTION('',(0.0560813448397477,0.998426202961924,1.1464801360602E-16));
#5674=DIRECTION('',(0.,1.14828730722317E-16,-1.));
#5675=DIRECTION('',(0.,1.,1.14828730722317E-16));
#5676=DIRECTION('',(0.,1.14828730722317E-16,-1.));
#5677=DIRECTION('',(0.,1.,1.14828730722317E-16));
#5678=DIRECTION('',(0.,1.14828730722317E-16,-1.));
#5679=DIRECTION('',(0.,1.,1.14828730722317E-16));
#5680=DIRECTION('',(0.,0.,1.));
#5681=DIRECTION('',(1.,0.,0.));
#5682=DIRECTION('',(0.,1.11917643611407E-16,-1.));
#5683=DIRECTION('',(0.,1.,1.11917643611407E-16));
#5684=DIRECTION('',(0.,0.,1.));
#5685=DIRECTION('',(0.,1.11917643611407E-16,-1.));
#5686=DIRECTION('',(0.,1.,1.11917643611407E-16));
#5687=DIRECTION('',(0.,7.65524871482112E-17,-1.));
#5688=DIRECTION('',(0.,1.,7.65524871482112E-17));
#5689=DIRECTION('',(0.,0.,1.));
#5690=DIRECTION('',(0.,1.14828730722317E-16,-1.));
#5691=DIRECTION('',(0.,1.,1.14828730722317E-16));
#5692=DIRECTION('',(0.,0.,1.));
#5693=DIRECTION('',(1.,0.,0.));
#5694=DIRECTION('',(0.,0.,-1.));
#5695=DIRECTION('',(-1.,0.,0.));
#5696=DIRECTION('',(0.,0.,-1.));
#5697=DIRECTION('',(-1.,0.,0.));
#5698=DIRECTION('',(0.,0.,1.));
#5699=DIRECTION('',(1.,0.,0.));
#5700=DIRECTION('',(0.,1.11917643611407E-16,-1.));
#5701=DIRECTION('',(0.,1.,1.11917643611407E-16));
#5702=DIRECTION('',(0.,0.,1.));
#5703=DIRECTION('',(0.,1.11917643611407E-16,-1.));
#5704=DIRECTION('',(0.,1.,1.11917643611407E-16));
#5705=DIRECTION('',(0.,1.14828730722317E-16,-1.));
#5706=DIRECTION('',(0.,1.,1.14828730722317E-16));
#5707=DIRECTION('',(0.,0.,1.));
#5708=DIRECTION('',(0.,7.65524871482112E-17,-1.));
#5709=DIRECTION('',(0.,1.,7.65524871482112E-17));
#5710=DIRECTION('',(-0.998426202961924,-0.0560813448397477,0.));
#5711=DIRECTION('',(0.0560813448397477,-0.998426202961924,0.));
#5712=DIRECTION('',(-0.0560813448397477,0.998426202961924,1.1464801360602E-16));
#5713=DIRECTION('',(-0.0560813448397477,0.998426202961924,7.643200907068E-17));
#5714=DIRECTION('',(-0.998426202961924,0.0560813448397477,0.));
#5715=DIRECTION('',(-0.0560813448397477,-0.998426202961924,0.));
#5716=DIRECTION('',(0.0560813448397477,0.998426202961924,1.1464801360602E-16));
#5717=DIRECTION('',(0.0560813448397477,0.998426202961924,7.643200907068E-17));
#5718=DIRECTION('',(0.,0.,1.));
#5719=DIRECTION('',(1.,0.,0.));
#5720=DIRECTION('',(0.,0.,-1.));
#5721=DIRECTION('',(-1.,0.,0.));
#5722=DIRECTION('',(0.,0.,1.));
#5723=DIRECTION('',(1.,0.,0.));
#5724=DIRECTION('',(-0.998426202961924,0.0560813448397478,0.));
#5725=DIRECTION('',(-0.0560813448397478,-0.998426202961924,0.));
#5726=DIRECTION('',(0.,0.,1.));
#5727=DIRECTION('',(-0.0560813448397478,-0.998426202961924,-7.643200907068E-17));
#5728=DIRECTION('',(0.,0.,1.));
#5729=DIRECTION('',(-0.0560813448397478,-0.998426202961924,0.));
#5730=DIRECTION('',(0.,0.,1.));
#5731=DIRECTION('',(1.,0.,0.));
#5732=DIRECTION('',(0.,7.65524871482112E-17,-1.));
#5733=DIRECTION('',(0.,1.,7.65524871482112E-17));
#5734=DIRECTION('',(0.,0.,1.));
#5735=DIRECTION('',(1.,0.,0.));
#5736=DIRECTION('',(0.,0.,1.));
#5737=DIRECTION('',(0.,7.65524871482112E-17,-1.));
#5738=DIRECTION('',(0.,1.,7.65524871482112E-17));
#5739=DIRECTION('',(-0.998426202961924,-0.0560813448397478,0.));
#5740=DIRECTION('',(0.0560813448397478,-0.998426202961924,0.));
#5741=DIRECTION('',(0.,0.,1.));
#5742=DIRECTION('',(0.0560813448397478,-0.998426202961924,-7.643200907068E-17));
#5743=DIRECTION('',(0.0560813448397478,-0.998426202961924,0.));
#5744=DIRECTION('',(0.,0.,1.));
#5745=DIRECTION('',(1.,0.,0.));
#5746=DIRECTION('',(0.,7.65524871482112E-17,-1.));
#5747=DIRECTION('',(0.,1.,7.65524871482112E-17));
#5748=DIRECTION('',(0.,7.65524871482112E-17,-1.));
#5749=DIRECTION('',(0.,1.,7.65524871482112E-17));
#5750=DIRECTION('',(0.,0.,1.));
#5751=DIRECTION('',(1.,0.,0.));
#5752=DIRECTION('',(0.,0.,1.));
#5753=DIRECTION('',(1.,0.,0.));
#5754=DIRECTION('',(0.0560813448397478,-0.998426202961924,0.));
#5755=DIRECTION('',(0.,0.,1.));
#5756=DIRECTION('',(1.,0.,0.));
#5757=DIRECTION('',(-0.0560813448397478,-0.998426202961924,0.));
#5758=DIRECTION('',(0.,0.,1.));
#5759=DIRECTION('',(1.,0.,0.));
#5760=DIRECTION('',(0.998426202961924,-0.0560813448397478,0.));
#5761=DIRECTION('',(0.0560813448397478,0.998426202961924,0.));
#5762=DIRECTION('',(0.,0.,-1.));
#5763=DIRECTION('',(-0.0560813448397478,-0.998426202961924,-1.1464801360602E-16));
#5764=DIRECTION('',(0.,0.,-1.));
#5765=DIRECTION('',(-0.0560813448397478,-0.998426202961924,0.));
#5766=DIRECTION('',(0.,0.,-1.));
#5767=DIRECTION('',(-1.,0.,0.));
#5768=DIRECTION('',(0.,0.,-1.));
#5769=DIRECTION('',(0.,1.14828730722317E-16,-1.));
#5770=DIRECTION('',(0.,1.,1.14828730722317E-16));
#5771=DIRECTION('',(0.,1.14828730722317E-16,-1.));
#5772=DIRECTION('',(0.,1.,1.14828730722317E-16));
#5773=DIRECTION('',(0.,0.,-1.));
#5774=DIRECTION('',(-1.,0.,0.));
#5775=DIRECTION('',(0.998426202961924,0.0560813448397478,0.));
#5776=DIRECTION('',(-0.0560813448397478,0.998426202961924,0.));
#5777=DIRECTION('',(0.,0.,-1.));
#5778=DIRECTION('',(0.0560813448397478,-0.998426202961924,-1.1464801360602E-16));
#5779=DIRECTION('',(0.0560813448397478,-0.998426202961924,0.));
#5780=DIRECTION('',(0.,0.,-1.));
#5781=DIRECTION('',(-1.,0.,0.));
#5782=DIRECTION('',(0.,1.14828730722317E-16,-1.));
#5783=DIRECTION('',(0.,1.,1.14828730722317E-16));
#5784=DIRECTION('',(0.,0.,-1.));
#5785=DIRECTION('',(-1.,0.,0.));
#5786=DIRECTION('',(0.,1.14828730722317E-16,-1.));
#5787=DIRECTION('',(0.,1.,1.14828730722317E-16));
#5788=DIRECTION('',(0.,0.,-1.));
#5789=DIRECTION('',(1.,0.,0.));
#5790=DIRECTION('',(0.0560813448397478,-0.998426202961924,0.));
#5791=DIRECTION('',(0.,0.,-1.));
#5792=DIRECTION('',(-1.,0.,0.));
#5793=DIRECTION('',(-0.0560813448397478,-0.998426202961924,0.));
#5794=DIRECTION('',(0.,0.,-1.));
#5795=DIRECTION('',(-1.,0.,0.));
#5796=DIRECTION('',(0.,1.14828730722317E-16,-1.));
#5797=DIRECTION('',(0.,1.,1.14828730722317E-16));
#5798=DIRECTION('',(0.,0.,-1.));
#5799=DIRECTION('',(-1.,0.,0.));
#5800=DIRECTION('',(1.,0.,0.));
#5801=DIRECTION('',(0.,0.,-1.));
#5802=DIRECTION('',(1.,0.,0.));
#5803=DIRECTION('',(0.,1.14828730722317E-16,-1.));
#5804=DIRECTION('',(0.,1.,1.14828730722317E-16));
#5805=DIRECTION('',(0.,0.,-1.));
#5806=DIRECTION('',(-1.,0.,0.));
#5807=DIRECTION('',(0.,7.65524871482112E-17,-1.));
#5808=DIRECTION('',(0.,1.,7.65524871482112E-17));
#5809=DIRECTION('',(0.,0.,1.));
#5810=DIRECTION('',(1.,0.,0.));
#5811=DIRECTION('',(-1.,0.,0.));
#5812=DIRECTION('',(0.,0.,1.));
#5813=DIRECTION('',(-1.,0.,0.));
#5814=DIRECTION('',(0.,7.65524871482112E-17,-1.));
#5815=DIRECTION('',(0.,1.,7.65524871482112E-17));
#5816=DIRECTION('',(0.,0.,1.));
#5817=DIRECTION('',(1.,0.,0.));
#5818=DIRECTION('',(0.,1.14828730722317E-16,-1.));
#5819=DIRECTION('',(0.,1.,1.14828730722317E-16));
#5820=DIRECTION('',(0.,1.11917643611407E-16,-1.));
#5821=DIRECTION('',(0.,1.,1.11917643611407E-16));
#5822=DIRECTION('',(0.,7.65524871482112E-17,-1.));
#5823=DIRECTION('',(0.,1.,7.65524871482112E-17));
#5824=DIRECTION('',(0.,-1.11917643611407E-16,1.));
#5825=DIRECTION('',(0.,-1.,-1.11917643611407E-16));
#5826=DIRECTION('',(0.,0.,1.));
#5827=DIRECTION('',(1.,0.,0.));
#5828=DIRECTION('',(-0.0560813448397478,0.998426202961924,0.));
#5829=DIRECTION('',(-0.998426202961924,-0.0560813448397478,0.));
#5830=DIRECTION('',(-0.0560813448397478,-0.998426202961924,0.));
#5831=DIRECTION('',(0.998426202961924,-0.0560813448397478,0.));
#5832=DIRECTION('',(0.,0.,1.));
#5833=DIRECTION('',(1.,0.,0.));
#5834=DIRECTION('',(0.,0.,1.));
#5835=DIRECTION('',(1.,0.,0.));
#5836=DIRECTION('',(0.,0.,1.));
#5837=DIRECTION('',(1.,0.,0.));
#5838=DIRECTION('',(0.,0.,1.));
#5839=DIRECTION('',(1.,0.,0.));
#5840=DIRECTION('',(0.,0.,-1.));
#5841=DIRECTION('',(1.,0.,0.));
#5842=DIRECTION('',(0.,0.,-1.));
#5843=DIRECTION('',(-1.,0.,0.));
#5844=DIRECTION('',(0.,0.,1.));
#5845=DIRECTION('',(1.,0.,0.));
#5846=DIRECTION('',(0.,1.14828730722317E-16,-1.));
#5847=DIRECTION('',(0.,1.,1.14828730722317E-16));
#5848=DIRECTION('',(0.983804137470403,-0.179246810560514,0.));
#5849=DIRECTION('',(0.179246810560514,0.983804137470403,0.));
#5850=DIRECTION('',(-0.0560813448397478,-0.998426202961924,-1.1464801360602E-16));
#5851=DIRECTION('',(0.998426202961924,-0.0560813448397478,0.));
#5852=DIRECTION('',(0.983804137470403,0.179246810560514,0.));
#5853=DIRECTION('',(-0.179246810560514,0.983804137470403,0.));
#5854=DIRECTION('',(0.,1.14828730722317E-16,-1.));
#5855=DIRECTION('',(0.,1.,1.14828730722317E-16));
#5856=DIRECTION('',(0.642413406945013,0.766358280817335,1.11440961830976E-15));
#5857=DIRECTION('',(-0.766358280817335,0.642413406945013,0.));
#5858=DIRECTION('',(0.,1.14828730722317E-16,-1.));
#5859=DIRECTION('',(0.,1.,1.14828730722317E-16));
#5860=DIRECTION('',(-0.0560813448397478,0.998426202961924,1.1464801360602E-16));
#5861=DIRECTION('',(-0.998426202961924,-0.0560813448397478,0.));
#5862=DIRECTION('',(0.999999999999785,6.01294052053665E-7,-2.61609735228368E-7));
#5863=DIRECTION('',(-6.01294052053685E-7,0.999999999999819,0.));
#5864=DIRECTION('',(0.,1.14828730722317E-16,-1.));
#5865=DIRECTION('',(0.,1.,1.14828730722317E-16));
#5866=DIRECTION('',(-0.642413406945014,0.766358280817334,0.));
#5867=DIRECTION('',(-0.766358280817334,-0.642413406945014,0.));
#5868=DIRECTION('',(0.,1.11917643611407E-16,-1.));
#5869=DIRECTION('',(0.,1.,1.11917643611407E-16));
#5870=DIRECTION('',(-0.552533958187431,-0.833490386897012,-9.32822800742734E-17));
#5871=DIRECTION('',(0.833490386897012,-0.552533958187431,0.));
#5872=DIRECTION('',(-0.928501017043572,-0.371329855181418,-4.15583623944693E-17));
#5873=DIRECTION('',(0.371329855181418,-0.928501017043572,0.));
#5874=DIRECTION('',(-0.535520596090342,-0.807825948455544,-0.246241605267967));
#5875=DIRECTION('',(0.833490386897012,-0.552533958187431,0.));
#5876=DIRECTION('',(0.197352473808094,0.980332597173952,0.));
#5877=DIRECTION('',(-0.980332597173952,0.197352473808094,0.));
#5878=DIRECTION('',(0.,1.14828730722317E-16,-1.));
#5879=DIRECTION('',(0.,1.,1.14828730722317E-16));
#5880=DIRECTION('',(0.0560813448397463,0.998426202961924,0.));
#5881=DIRECTION('',(-0.998426202961924,0.0560813448397463,0.));
#5882=DIRECTION('',(0.0560813448397477,0.998426202961924,1.1464801360602E-16));
#5883=DIRECTION('',(-0.998426202961924,0.0560813448397477,0.));
#5884=DIRECTION('',(0.0560813448397463,0.998426202961924,0.));
#5885=DIRECTION('',(-0.998426202961924,0.0560813448397463,0.));
#5886=DIRECTION('',(0.,1.14828730722317E-16,-1.));
#5887=DIRECTION('',(0.,1.,1.14828730722317E-16));
#5888=DIRECTION('',(-0.0527919210430931,0.998605534268952,0.));
#5889=DIRECTION('',(-0.998605534268952,-0.0527919210430931,0.));
#5890=DIRECTION('',(0.234713071091589,-0.914083668468321,0.330697477006177));
#5891=DIRECTION('',(0.,-0.340201097913941,-0.940352706689436));
#5892=DIRECTION('',(0.,1.11917643611407E-16,-1.));
#5893=DIRECTION('',(0.,1.,1.11917643611407E-16));
#5894=DIRECTION('',(-0.928501017043572,0.371329855181418,4.15583623944693E-17));
#5895=DIRECTION('',(-0.371329855181418,-0.928501017043572,0.));
#5896=DIRECTION('',(-0.552533958187431,0.833490386897012,9.32822800742734E-17));
#5897=DIRECTION('',(-0.833490386897012,-0.552533958187431,0.));
#5898=DIRECTION('',(-0.535520596090342,0.807825948455544,0.246241605267967));
#5899=DIRECTION('',(-0.833490386897012,-0.552533958187431,0.));
#5900=DIRECTION('',(-0.197352473808102,0.98033259717395,0.));
#5901=DIRECTION('',(-0.98033259717395,-0.197352473808102,0.));
#5902=DIRECTION('',(0.,1.14828730722317E-16,-1.));
#5903=DIRECTION('',(0.,1.,1.14828730722317E-16));
#5904=DIRECTION('',(-0.05608134483975,0.998426202961924,3.85312924844834E-15));
#5905=DIRECTION('',(-0.998426202961924,-0.05608134483975,0.));
#5906=DIRECTION('',(0.0560813448397477,-0.998426202961924,-1.1464801360602E-16));
#5907=DIRECTION('',(0.998426202961924,0.0560813448397477,0.));
#5908=DIRECTION('',(-0.0560813448397466,0.998426202961924,0.));
#5909=DIRECTION('',(-0.998426202961924,-0.0560813448397466,0.));
#5910=DIRECTION('',(0.,1.14828730722317E-16,-1.));
#5911=DIRECTION('',(0.,1.,1.14828730722317E-16));
#5912=DIRECTION('',(0.0527919210430855,0.998605534268953,7.6618529323497E-15));
#5913=DIRECTION('',(-0.998605534268953,0.0527919210430855,0.));
#5914=DIRECTION('',(0.234713071091591,0.914083668468322,-0.330697477006173));
#5915=DIRECTION('',(0.,0.340201097913937,0.940352706689437));
#5916=DIRECTION('',(0.,7.65524871482112E-17,-1.));
#5917=DIRECTION('',(0.,1.,7.65524871482112E-17));
#5918=DIRECTION('',(-0.9838041374704,-0.17924681056053,0.));
#5919=DIRECTION('',(0.17924681056053,-0.9838041374704,0.));
#5920=DIRECTION('',(-0.0560813448397478,0.998426202961924,7.643200907068E-17));
#5921=DIRECTION('',(-0.998426202961924,-0.0560813448397478,0.));
#5922=DIRECTION('',(-0.9838041374704,0.17924681056053,0.));
#5923=DIRECTION('',(-0.17924681056053,-0.9838041374704,0.));
#5924=DIRECTION('',(0.,7.65524871482112E-17,-1.));
#5925=DIRECTION('',(0.,1.,7.65524871482112E-17));
#5926=DIRECTION('',(-0.642413406945013,0.766358280817335,0.));
#5927=DIRECTION('',(-0.766358280817335,-0.642413406945013,0.));
#5928=DIRECTION('',(0.,7.65524871482112E-17,-1.));
#5929=DIRECTION('',(0.,1.,7.65524871482112E-17));
#5930=DIRECTION('',(-0.0560813448397478,-0.998426202961924,-7.643200907068E-17));
#5931=DIRECTION('',(0.998426202961924,-0.0560813448397478,0.));
#5932=DIRECTION('',(0.999999999999784,6.04763510871776E-7,2.58438346553984E-7));
#5933=DIRECTION('',(-6.04763510871797E-7,0.999999999999817,0.));
#5934=DIRECTION('',(0.,7.65524871482112E-17,-1.));
#5935=DIRECTION('',(0.,1.,7.65524871482112E-17));
#5936=DIRECTION('',(0.642413406945013,0.766358280817335,0.));
#5937=DIRECTION('',(-0.766358280817335,0.642413406945013,0.));
#5938=DIRECTION('',(0.,1.11917643611407E-16,-1.));
#5939=DIRECTION('',(0.,1.,1.11917643611407E-16));
#5940=DIRECTION('',(-0.552533958187431,0.833490386897012,9.32822800742734E-17));
#5941=DIRECTION('',(-0.833490386897012,-0.552533958187431,0.));
#5942=DIRECTION('',(-0.928501017043572,0.371329855181418,4.15583623944693E-17));
#5943=DIRECTION('',(-0.371329855181418,-0.928501017043572,0.));
#5944=DIRECTION('',(0.535520596090342,-0.807825948455544,0.246241605267969));
#5945=DIRECTION('',(0.833490386897012,0.552533958187431,0.));
#5946=DIRECTION('',(-0.197352473808615,0.980332597173847,-2.23319085694374E-13));
#5947=DIRECTION('',(-0.980332597173847,-0.197352473808615,0.));
#5948=DIRECTION('',(0.,7.65524871482112E-17,-1.));
#5949=DIRECTION('',(0.,1.,7.65524871482112E-17));
#5950=DIRECTION('',(-0.0560813448397463,0.998426202961924,0.));
#5951=DIRECTION('',(-0.998426202961924,-0.0560813448397463,0.));
#5952=DIRECTION('',(-0.0560813448397477,0.998426202961924,7.643200907068E-17));
#5953=DIRECTION('',(-0.998426202961924,-0.0560813448397477,0.));
#5954=DIRECTION('',(-0.0560813448397463,0.998426202961924,0.));
#5955=DIRECTION('',(-0.998426202961924,-0.0560813448397463,0.));
#5956=DIRECTION('',(0.,7.65524871482112E-17,-1.));
#5957=DIRECTION('',(0.,1.,7.65524871482112E-17));
#5958=DIRECTION('',(0.0527919210430856,0.998605534268953,0.));
#5959=DIRECTION('',(-0.998605534268953,0.0527919210430856,0.));
#5960=DIRECTION('',(-0.23471307109159,-0.914083668468321,-0.330697477006176));
#5961=DIRECTION('',(0.,0.34020109791394,-0.940352706689436));
#5962=DIRECTION('',(0.,1.11917643611407E-16,-1.));
#5963=DIRECTION('',(0.,1.,1.11917643611407E-16));
#5964=DIRECTION('',(-0.552533958187431,-0.833490386897012,-9.32822800742734E-17));
#5965=DIRECTION('',(0.833490386897012,-0.552533958187431,0.));
#5966=DIRECTION('',(-0.928501017043572,-0.371329855181418,-4.15583623944693E-17));
#5967=DIRECTION('',(0.371329855181418,-0.928501017043572,0.));
#5968=DIRECTION('',(0.535520596090342,0.807825948455544,-0.246241605267969));
#5969=DIRECTION('',(-0.833490386897011,0.552533958187431,0.));
#5970=DIRECTION('',(0.197352473808095,0.980332597173951,0.));
#5971=DIRECTION('',(-0.980332597173952,0.197352473808095,0.));
#5972=DIRECTION('',(0.,7.65524871482112E-17,-1.));
#5973=DIRECTION('',(0.,1.,7.65524871482112E-17));
#5974=DIRECTION('',(0.05608134483975,0.998426202961924,-3.85312924844833E-15));
#5975=DIRECTION('',(-0.998426202961924,0.05608134483975,0.));
#5976=DIRECTION('',(-0.0560813448397477,-0.998426202961924,-7.643200907068E-17));
#5977=DIRECTION('',(0.998426202961924,-0.0560813448397477,0.));
#5978=DIRECTION('',(0.0560813448397466,0.998426202961924,0.));
#5979=DIRECTION('',(-0.998426202961924,0.0560813448397466,0.));
#5980=DIRECTION('',(0.,7.65524871482112E-17,-1.));
#5981=DIRECTION('',(0.,1.,7.65524871482112E-17));
#5982=DIRECTION('',(-0.0527919210431341,0.99860553426895,-2.21826550717474E-13));
#5983=DIRECTION('',(-0.99860553426895,-0.0527919210431341,0.));
#5984=DIRECTION('',(-0.234713071091591,0.914083668468323,0.330697477006171));
#5985=DIRECTION('',(0.,-0.340201097913935,0.940352706689438));
#5986=DIRECTION('',(0.,0.,-1.));
#5987=DIRECTION('',(-1.,0.,0.));
#5988=DIRECTION('',(0.0560813448397478,0.998426202961924,0.));
#5989=DIRECTION('',(-0.998426202961924,0.0560813448397478,0.));
#5990=DIRECTION('',(0.0560813448397478,-0.998426202961924,0.));
#5991=DIRECTION('',(0.998426202961924,0.0560813448397478,0.));
#5992=DIRECTION('',(0.,0.,-1.));
#5993=DIRECTION('',(-1.,0.,0.));
#5994=DIRECTION('',(0.,0.,1.));
#5995=DIRECTION('',(1.,0.,0.));
#5996=DIRECTION('',(0.756219796281132,0.654317674919854,-2.62366446721458E-15));
#5997=DIRECTION('',(-0.654317674919854,0.756219796281132,0.));
#5998=DIRECTION('',(0.,-1.11917643611407E-16,1.));
#5999=DIRECTION('',(0.,-1.,-1.11917643611407E-16));
#6000=DIRECTION('',(0.756219796281135,-0.65431767491985,1.91657645850553E-15));
#6001=DIRECTION('',(0.65431767491985,0.756219796281135,0.));
#6002=DIRECTION('',(0.,0.,1.));
#6003=DIRECTION('',(1.,0.,0.));
#6004=DIRECTION('',(-1.,0.,0.));
#6005=DIRECTION('',(0.,0.,1.));
#6006=DIRECTION('',(0.,0.,1.));
#6007=DIRECTION('',(1.,0.,0.));
#6008=DIRECTION('',(0.,0.,1.));
#6009=DIRECTION('',(1.,0.,0.));
#6010=DIRECTION('',(-3.46944695195364E-15,-1.38751515677455E-15,1.));
#6011=DIRECTION('',(1.,0.,3.46944695195364E-15));
#6012=DIRECTION('',(-1.,0.,0.));
#6013=DIRECTION('',(0.,0.,1.));
#6014=DIRECTION('',(-1.,0.,0.));
#6015=DIRECTION('',(0.,0.,1.));
#6016=DIRECTION('',(0.,-1.86830541284738E-15,1.));
#6017=DIRECTION('',(0.,-1.,-1.86830541284738E-15));
#6018=DIRECTION('',(0.,0.,1.));
#6019=DIRECTION('',(1.,0.,0.));
#6020=DIRECTION('',(0.,0.,1.));
#6021=DIRECTION('',(1.,0.,0.));
#6022=DIRECTION('',(-1.,0.,0.));
#6023=DIRECTION('',(0.,0.,1.));
#6024=DIRECTION('',(0.,0.,1.));
#6025=DIRECTION('',(1.,0.,0.));
#6026=DIRECTION('',(-0.756219796281137,0.654317674919848,2.62366446721458E-15));
#6027=DIRECTION('',(-0.654317674919848,-0.756219796281137,0.));
#6028=DIRECTION('',(0.,-1.11917643611407E-16,1.));
#6029=DIRECTION('',(0.,-1.,-1.11917643611407E-16));
#6030=DIRECTION('',(-0.756219796281092,-0.6543176749199,0.));
#6031=DIRECTION('',(0.6543176749199,-0.756219796281092,0.));
#6032=DIRECTION('',(0.,0.,1.));
#6033=DIRECTION('',(1.,0.,0.));
#6034=DIRECTION('',(0.,0.,-1.));
#6035=DIRECTION('',(-1.,0.,0.));
#6036=DIRECTION('',(0.299336048990059,-0.954147750495184,0.));
#6037=DIRECTION('',(0.954147750495185,0.299336048990059,0.));
#6038=DIRECTION('',(-0.299336048990059,-0.954147750495184,0.));
#6039=DIRECTION('',(0.954147750495185,-0.299336048990059,0.));
#6040=DIRECTION('',(0.,0.,-1.));
#6041=DIRECTION('',(-1.,0.,0.));
#6042=DIRECTION('',(-0.248706066143853,-0.968579006928836,0.));
#6043=DIRECTION('',(0.968579006928836,-0.248706066143853,0.));
#6044=DIRECTION('',(0.,0.,-1.));
#6045=DIRECTION('',(-1.,0.,0.));
#6046=DIRECTION('',(0.248706066143863,-0.968579006928833,0.));
#6047=DIRECTION('',(0.968579006928833,0.248706066143863,0.));
#6048=DIRECTION('',(0.,0.,-1.));
#6049=DIRECTION('',(-1.,0.,0.));
#6050=DIRECTION('',(-0.517694816437262,-0.855565355209051,0.));
#6051=DIRECTION('',(0.855565355209051,-0.517694816437262,0.));
#6052=DIRECTION('',(0.,0.,-1.));
#6053=DIRECTION('',(-1.,0.,0.));
#6054=DIRECTION('',(0.517694816437954,-0.855565355208632,8.98057351466427E-16));
#6055=DIRECTION('',(0.855565355208632,0.517694816437955,0.));
#6056=DIRECTION('',(0.,0.,1.));
#6057=DIRECTION('',(1.,0.,0.));
#6058=DIRECTION('',(0.,0.,1.));
#6059=DIRECTION('',(1.,0.,0.));
#6060=DIRECTION('',(1.,0.,0.));
#6061=DIRECTION('',(0.,0.,-1.));
#6062=DIRECTION('',(0.,0.,-1.));
#6063=DIRECTION('',(-1.,0.,0.));
#6064=DIRECTION('',(0.,0.,-1.));
#6065=DIRECTION('',(-1.,0.,0.));
#6066=DIRECTION('',(0.,0.,1.));
#6067=DIRECTION('',(1.,0.,0.));
#6068=DIRECTION('',(0.,0.,-1.));
#6069=DIRECTION('',(-1.,0.,0.));
#6070=DIRECTION('',(0.299336048990059,-0.954147750495184,0.));
#6071=DIRECTION('',(0.954147750495185,0.299336048990059,0.));
#6072=DIRECTION('',(-0.299336048990059,-0.954147750495185,0.));
#6073=DIRECTION('',(0.954147750495185,-0.299336048990059,0.));
#6074=DIRECTION('',(0.,0.,-1.));
#6075=DIRECTION('',(-1.,0.,0.));
#6076=DIRECTION('',(-0.248706066143425,-0.968579006928946,0.));
#6077=DIRECTION('',(0.968579006928946,-0.248706066143425,0.));
#6078=DIRECTION('',(0.,0.,-1.));
#6079=DIRECTION('',(-1.,0.,0.));
#6080=DIRECTION('',(0.24870606614387,-0.968579006928831,0.));
#6081=DIRECTION('',(0.968579006928831,0.24870606614387,0.));
#6082=DIRECTION('',(0.,0.,-1.));
#6083=DIRECTION('',(-1.,0.,0.));
#6084=DIRECTION('',(-0.517694816437967,-0.855565355208624,0.));
#6085=DIRECTION('',(0.855565355208624,-0.517694816437967,0.));
#6086=DIRECTION('',(0.,0.,-1.));
#6087=DIRECTION('',(-1.,0.,0.));
#6088=DIRECTION('',(0.517694816437267,-0.855565355209048,0.));
#6089=DIRECTION('',(0.855565355209048,0.517694816437267,0.));
#6090=DIRECTION('',(0.,0.,1.));
#6091=DIRECTION('',(1.,0.,0.));
#6092=DIRECTION('',(0.,0.,1.));
#6093=DIRECTION('',(1.,0.,0.));
#6094=DIRECTION('',(-1.,0.,0.));
#6095=DIRECTION('',(0.,0.,1.));
#6096=DIRECTION('',(0.,0.,-1.));
#6097=DIRECTION('',(-1.,0.,0.));
#6098=DIRECTION('',(0.,-1.,0.));
#6099=DIRECTION('',(1.,0.,0.));
#6100=DIRECTION('',(0.,-1.,0.));
#6101=DIRECTION('',(1.,0.,0.));
#6102=DIRECTION('',(-1.,-2.56739074444557E-16,1.82918119333768E-16));
#6103=DIRECTION('',(2.56739074444557E-16,-1.,-4.5102810375397E-16));
#6104=DIRECTION('',(0.,-1.,0.));
#6105=DIRECTION('',(1.,0.,0.));
#6106=DIRECTION('',(0.,0.,-1.));
#6107=DIRECTION('',(1.,0.,0.));
#6108=DIRECTION('',(0.,0.,-1.));
#6109=DIRECTION('',(-1.,0.,0.));
#6110=DIRECTION('',(0.,0.,-1.));
#6111=DIRECTION('',(-1.,0.,0.));
#6112=DIRECTION('',(0.,0.,1.));
#6113=DIRECTION('',(1.,0.,0.));
#6114=DIRECTION('',(0.,0.,-1.));
#6115=DIRECTION('',(-1.,0.,0.));
#6116=DIRECTION('',(0.,0.,-1.));
#6117=DIRECTION('',(0.,0.,-1.));
#6118=DIRECTION('',(-1.,0.,0.));
#6119=DIRECTION('',(0.,0.,1.));
#6120=DIRECTION('',(1.,0.,0.));
#6121=DIRECTION('',(0.,0.,-1.));
#6122=DIRECTION('',(0.,0.,-1.));
#6123=DIRECTION('',(-1.,0.,0.));
#6124=DIRECTION('',(0.,0.,-1.));
#6125=DIRECTION('',(1.,0.,0.));
#6126=DIRECTION('',(-1.,0.,0.));
#6127=DIRECTION('',(0.,0.,1.));
#6128=DIRECTION('',(1.,0.,0.));
#6129=DIRECTION('',(1.,0.,0.));
#6130=DIRECTION('',(0.,-1.,0.));
#6131=DIRECTION('',(1.,0.,0.));
#6132=DIRECTION('',(-1.,-8.32667268468852E-17,1.216857793764E-16));
#6133=DIRECTION('',(8.32667268468853E-17,-1.,3.7148595991706E-16));
#6134=DIRECTION('',(0.,0.,-1.));
#6135=DIRECTION('',(-1.,0.,0.));
#6136=DIRECTION('',(0.,0.,1.));
#6137=DIRECTION('',(1.,-6.12323399573677E-17,0.));
#6138=DIRECTION('',(0.,0.,1.));
#6139=DIRECTION('',(1.,-6.12323399573677E-17,0.));
#6140=DIRECTION('',(0.,0.,-1.));
#6141=DIRECTION('',(-1.,0.,0.));
#6142=DIRECTION('',(0.,0.,1.));
#6143=DIRECTION('',(1.,-6.12323399573677E-17,0.));
#6144=DIRECTION('',(0.,0.,1.));
#6145=DIRECTION('',(1.,-6.12323399573677E-17,0.));
#6146=DIRECTION('',(0.,0.,1.));
#6147=DIRECTION('',(1.,0.,0.));
#6148=DIRECTION('',(0.,0.,1.));
#6149=DIRECTION('',(1.,0.,0.));
#6150=DIRECTION('',(1.,3.05311331771918E-16,-1.21685779376401E-16));
#6151=DIRECTION('',(3.05311331771918E-16,-1.,-5.12260443711338E-16));
#6152=DIRECTION('',(0.,0.,-1.));
#6153=DIRECTION('',(1.,0.,0.));
#6154=DIRECTION('',(0.,0.,1.));
#6155=DIRECTION('',(-3.22276666936548E-17,-1.,0.));
#6156=DIRECTION('',(0.,0.,1.));
#6157=DIRECTION('',(1.,0.,0.));
#6158=DIRECTION('',(0.,0.,1.));
#6159=DIRECTION('',(1.,0.,0.));
#6160=DIRECTION('',(0.,0.,-1.));
#6161=DIRECTION('',(0.,-1.,0.));
#6162=DIRECTION('',(-0.165120262618152,-0.986273440214686,0.));
#6163=DIRECTION('',(0.,0.,-1.));
#6164=DIRECTION('',(0.997579197588362,0.0695395178223138,0.));
#6165=DIRECTION('',(-0.165120262618151,0.986273440214686,0.));
#6166=DIRECTION('',(0.,0.,-1.));
#6167=DIRECTION('',(-0.965831339887295,0.259171416038716,0.));
#6168=DIRECTION('',(0.,0.,-1.));
#6169=DIRECTION('',(1.,0.,0.));
#6170=DIRECTION('',(0.,0.,1.));
#6171=DIRECTION('',(1.,0.,0.));
#6172=DIRECTION('',(0.,0.,1.));
#6173=DIRECTION('',(1.,0.,0.));
#6174=DIRECTION('',(0.,0.,1.));
#6175=DIRECTION('',(1.,0.,0.));
#6176=DIRECTION('',(-0.165120262618152,-0.986273440214686,0.));
#6177=DIRECTION('',(0.,0.,1.));
#6178=DIRECTION('',(0.986273440214687,0.165120262618151,0.));
#6179=DIRECTION('',(-0.165120262618151,0.986273440214686,0.));
#6180=DIRECTION('',(1.,0.,0.));
#6181=DIRECTION('',(1.,0.,0.));
#6182=DIRECTION('',(-0.986273440214686,0.165120262618152,0.));
#6183=DIRECTION('',(-0.165120262618152,-0.986273440214686,0.));
#6184=DIRECTION('',(-3.5527136788005E-16,-7.105427357601E-16,-1.));
#6185=DIRECTION('',(0.,0.,1.));
#6186=DIRECTION('',(-0.143488198627506,-0.85706379729923,0.494826014083393));
#6187=DIRECTION('',(0.986273440214686,-0.165120262618152,6.12323399573663E-17));
#6188=DIRECTION('',(-0.165120262618152,-0.986273440214686,-1.60794481439885E-13));
#6189=DIRECTION('',(-0.165120262618152,-0.986273440214686,0.));
#6190=DIRECTION('',(0.,0.,-1.));
#6191=DIRECTION('',(1.,0.,0.));
#6192=DIRECTION('',(0.,0.,1.));
#6193=DIRECTION('',(0.986273440214686,0.165120262618151,0.));
#6194=DIRECTION('',(-0.165120262618151,0.986273440214686,0.));
#6195=DIRECTION('',(-3.5527136788005E-16,7.105427357601E-16,-1.));
#6196=DIRECTION('',(-0.165120262618151,0.986273440214686,0.));
#6197=DIRECTION('',(0.986273440214686,0.165120262618152,6.12323399573648E-17));
#6198=DIRECTION('',(0.165120262618152,-0.986273440214686,1.37737697698504E-13));
#6199=DIRECTION('',(0.143488198627506,-0.85706379729923,0.494826014083392));
#6200=DIRECTION('',(0.,0.5,0.866025403784439));
#6201=DIRECTION('',(0.,-0.866025403784439,0.5));
#6202=DIRECTION('',(1.,0.,0.));
#6203=DIRECTION('',(0.,0.,-1.));
#6204=DIRECTION('',(-1.,0.,0.));
#6205=DIRECTION('',(0.,0.,1.));
#6206=DIRECTION('',(1.,0.,0.));
#6207=DIRECTION('',(0.,0.,1.));
#6208=DIRECTION('',(1.,0.,0.));
#6209=DIRECTION('',(-1.,0.,0.));
#6210=DIRECTION('',(0.,0.,-1.));
#6211=DIRECTION('',(1.,0.,0.));
#6212=DIRECTION('',(0.,0.,1.));
#6213=DIRECTION('',(1.,0.,0.));
#6214=DIRECTION('',(0.,0.,-1.));
#6215=DIRECTION('',(0.986273440214686,0.165120262618156,0.));
#6216=DIRECTION('',(0.,0.,1.));
#6217=DIRECTION('',(-0.939132344209142,-0.343555585109953,0.));
#6218=DIRECTION('',(0.,0.,-1.));
#6219=DIRECTION('',(-0.93913234420914,-0.343555585109957,0.));
#6220=DIRECTION('',(-4.7167604994452E-18,4.7167604994452E-18,1.));
#6221=DIRECTION('',(-0.939132344209142,-0.343555585109952,-2.80919293170665E-18));
#6222=DIRECTION('',(0.,0.,-1.));
#6223=DIRECTION('',(0.,0.,-1.));
#6224=DIRECTION('',(1.,-6.12323399573677E-17,0.));
#6225=DIRECTION('',(0.,0.,-1.));
#6226=DIRECTION('',(1.,-6.12323399573677E-17,0.));
#6227=DIRECTION('',(-2.46519032881566E-34,-9.43119924304831E-18,1.));
#6228=DIRECTION('',(0.986273440214686,0.165120262618152,1.55728209581625E-18));
#6229=DIRECTION('',(0.,0.,-1.));
#6230=DIRECTION('',(0.,-0.888557159765258,-0.458765924878798));
#6231=DIRECTION('',(0.,-0.458765924878798,0.888557159765258));
#6232=DIRECTION('',(-7.09909674989915E-15,0.009750455400229,-0.99995246317987));
#6233=DIRECTION('',(-1.52981362508847E-13,0.99995246317987,0.009750455400229));
#6234=DIRECTION('',(-1.97831778091143E-14,0.236053850037173,-0.971739975447459));
#6235=DIRECTION('',(-5.82449999783108E-15,0.971739975447459,0.236053850037173));
#6236=DIRECTION('',(0.,-0.897334135151735,0.441351843648));
#6237=DIRECTION('',(0.,0.441351843648,0.897334135151735));
#6238=DIRECTION('',(-3.30575397759658E-16,-0.226567721496539,-0.973995414555873));
#6239=DIRECTION('',(-9.67639922184483E-15,0.973995414555873,-0.226567721496539));
#6240=DIRECTION('',(0.,0.,-1.));
#6241=DIRECTION('',(1.,0.,0.));
#6242=DIRECTION('',(0.,0.,1.));
#6243=DIRECTION('',(0.,-1.,0.));
#6244=DIRECTION('',(0.,0.,1.));
#6245=DIRECTION('',(5.73018335290403E-17,1.,0.));
#6246=DIRECTION('',(0.,0.,1.));
#6247=DIRECTION('',(-1.,0.,0.));
#6248=DIRECTION('',(0.,-1.48882899694033E-16,1.));
#6249=DIRECTION('',(0.,-1.,-1.48882899694033E-16));
#6250=DIRECTION('',(0.,0.,1.));
#6251=DIRECTION('',(-1.,-1.8367567571222E-16,0.));
#6252=DIRECTION('',(0.101700025524789,0.994815108822059,-6.37778367330008E-5));
#6253=DIRECTION('',(-0.973565999163698,0.0995145471552375,-0.205587208203424));
#6254=DIRECTION('',(-0.101703879828654,0.994814714812882,-6.34000234451596E-5));
#6255=DIRECTION('',(0.994735072765686,0.101696543707177,0.0126470553038893));
#6256=DIRECTION('',(-0.101686733058552,-0.99481646753779,6.50808128760761E-5));
#6257=DIRECTION('',(0.994736828143844,-0.101679419936604,-0.0126466713280615));
#6258=DIRECTION('',(0.101687994499013,-0.994816338604938,6.49571619446657E-5));
#6259=DIRECTION('',(-0.973567282668449,-0.0995025376029421,0.205586942990423));
#6260=DIRECTION('',(0.,-1.,0.));
#6261=DIRECTION('',(0.,0.,1.));
#6262=DIRECTION('',(0.,-0.971739975447459,-0.236053850037172));
#6263=DIRECTION('',(0.,-0.236053850037173,0.971739975447459));
#6264=DIRECTION('',(3.44043640502547E-16,0.236053850037172,-0.971739975447459));
#6265=DIRECTION('',(3.64515562786427E-14,0.971739975447459,0.236053850037172));
#6266=DIRECTION('',(0.,-0.971739975447459,-0.236053850037172));
#6267=DIRECTION('',(0.,0.236053850037173,-0.971739975447459));
#6268=DIRECTION('',(0.,0.,-1.));
#6269=DIRECTION('',(1.,0.,0.));
#6270=DIRECTION('',(0.,0.,-1.));
#6271=DIRECTION('',(-1.,0.,0.));
#6272=DIRECTION('',(-2.45014736469E-16,-2.45014736469E-16,-1.));
#6273=DIRECTION('',(1.,-1.8367567571222E-16,-2.45014736469E-16));
#6274=DIRECTION('',(0.101527794842484,0.994832700123817,7.50917920324775E-5));
#6275=DIRECTION('',(-0.994759690413714,0.101521257725348,-0.0121075413637714));
#6276=DIRECTION('',(0.,-1.,0.));
#6277=DIRECTION('',(0.,0.,1.));
#6278=DIRECTION('',(0.,-0.973995414555873,0.226567721496538));
#6279=DIRECTION('',(0.,-0.226567721496537,-0.973995414555873));
#6280=DIRECTION('',(0.,0.,-1.));
#6281=DIRECTION('',(0.,-1.,0.));
#6282=DIRECTION('',(0.,0.,-1.));
#6283=DIRECTION('',(-1.,0.,0.));
#6284=DIRECTION('',(-0.165120262618151,0.986273440214686,0.));
#6285=DIRECTION('',(0.,0.,-1.));
#6286=DIRECTION('',(-0.986273440214686,0.165120262618152,0.));
#6287=DIRECTION('',(-0.165120262618152,-0.986273440214686,0.));
#6288=DIRECTION('',(-1.,0.,0.));
#6289=DIRECTION('',(-1.,0.,0.));
#6290=DIRECTION('',(0.,0.,-1.));
#6291=DIRECTION('',(0.,-1.,0.));
#6292=DIRECTION('',(0.,0.,1.));
#6293=DIRECTION('',(1.22464679914735E-16,1.,0.));
#6294=DIRECTION('',(0.,-0.888557159765256,-0.4587659248788));
#6295=DIRECTION('',(0.,-0.4587659248788,0.888557159765256));
#6296=DIRECTION('',(0.,-0.888557159765256,-0.4587659248788));
#6297=DIRECTION('',(0.,-0.4587659248788,0.888557159765256));
#6298=DIRECTION('',(0.,-0.888557159765258,-0.458765924878798));
#6299=DIRECTION('',(0.,-0.458765924878798,0.888557159765258));
#6300=DIRECTION('',(0.,-1.48882899694033E-16,1.));
#6301=DIRECTION('',(0.,-1.,-1.48882899694033E-16));
#6302=DIRECTION('',(0.,-0.897334135151735,0.441351843648));
#6303=DIRECTION('',(0.,0.441351843648,0.897334135151735));
#6304=DIRECTION('',(0.986273440214686,0.165120262618151,0.));
#6305=DIRECTION('',(0.165120262618151,-0.986273440214686,0.));
#6306=DIRECTION('',(0.986273440214687,0.165120262618151,-6.12323399573688E-17));
#6307=DIRECTION('',(-0.165120262618151,0.986273440214687,5.54312453933483E-14));
#6308=DIRECTION('',(-0.165120262618151,0.986273440214687,0.));
#6309=DIRECTION('',(0.,0.,1.));
#6310=DIRECTION('',(0.165120262618151,-0.986273440214686,0.));
#6311=DIRECTION('',(0.,0.,-1.));
#6312=DIRECTION('',(-0.143488198627506,0.85706379729923,0.494826014083392));
#6313=DIRECTION('',(0.,0.,1.));
#6314=DIRECTION('',(-1.,0.,0.));
#6315=DIRECTION('',(0.,0.,-1.));
#6316=DIRECTION('',(-0.986273440214686,0.165120262618152,0.));
#6317=DIRECTION('',(0.165120262618152,0.986273440214686,0.));
#6318=DIRECTION('',(0.165120262618152,0.986273440214686,0.));
#6319=DIRECTION('',(0.,7.9356111150447E-16,1.));
#6320=DIRECTION('',(-0.165120262618152,-0.986273440214686,0.));
#6321=DIRECTION('',(0.986273440214686,-0.165120262618152,6.12323399573693E-17));
#6322=DIRECTION('',(-0.165120262618152,-0.986273440214686,1.41223724344064E-13));
#6323=DIRECTION('',(0.143488198627506,0.85706379729923,0.494826014083392));
#6324=DIRECTION('',(0.,0.5,-0.866025403784439));
#6325=DIRECTION('',(0.,0.866025403784439,0.5));
#6326=DIRECTION('',(1.,0.,0.));
#6327=DIRECTION('',(0.,0.,1.));
#6328=DIRECTION('',(0.,-1.,0.));
#6329=DIRECTION('',(0.,0.,-1.));
#6330=DIRECTION('',(0.,-1.,0.));
#6331=DIRECTION('',(-1.,0.,0.));
#6332=DIRECTION('',(0.,0.,-1.));
#6333=DIRECTION('',(1.,0.,0.));
#6334=DIRECTION('',(0.,0.,-1.));
#6335=DIRECTION('',(-1.,0.,0.));
#6336=DIRECTION('',(0.,0.,1.));
#6337=DIRECTION('',(-0.986273440214685,0.16512026261816,0.));
#6338=DIRECTION('',(0.,0.,-1.));
#6339=DIRECTION('',(0.939132344209141,-0.343555585109954,0.));
#6340=DIRECTION('',(0.,0.,1.));
#6341=DIRECTION('',(0.939132344209136,-0.343555585109968,0.));
#6342=DIRECTION('',(0.,0.,-1.));
#6343=DIRECTION('',(0.939132344209141,-0.343555585109954,0.));
#6344=DIRECTION('',(0.,0.,1.));
#6345=DIRECTION('',(0.,0.,1.));
#6346=DIRECTION('',(0.,1.,0.));
#6347=DIRECTION('',(0.,0.,-1.));
#6348=DIRECTION('',(0.997579197588364,0.0695395178222898,0.));
#6349=DIRECTION('',(0.,0.,-1.));
#6350=DIRECTION('',(-1.,0.,0.));
#6351=DIRECTION('',(0.,0.,-1.));
#6352=DIRECTION('',(-0.965831339887311,0.259171416038655,0.));
#6353=DIRECTION('',(0.,0.,1.));
#6354=DIRECTION('',(0.,1.,0.));
#6355=DIRECTION('',(0.,0.,-1.));
#6356=DIRECTION('',(-0.986273440214686,0.165120262618152,0.));
#6357=DIRECTION('',(0.,0.,1.));
#6358=DIRECTION('',(0.,0.,1.));
#6359=DIRECTION('',(-1.,0.,0.));
#6360=DIRECTION('',(0.,-1.48882899694033E-16,1.));
#6361=DIRECTION('',(0.,-1.,-1.48882899694033E-16));
#6362=DIRECTION('',(0.,0.,-1.));
#6363=DIRECTION('',(-1.,0.,0.));
#6364=DIRECTION('',(0.,0.,1.));
#6365=DIRECTION('',(1.,0.,0.));
#6366=DIRECTION('',(0.,0.,1.));
#6367=DIRECTION('',(1.,0.,0.));
#6368=DIRECTION('',(1.,1.59594559789866E-16,-1.21685779376401E-16));
#6369=DIRECTION('',(-1.59594559789866E-16,1.,-3.71485959917063E-16));
#6370=DIRECTION('',(0.,0.,-1.));
#6371=DIRECTION('',(1.,0.,0.));
#6372=DIRECTION('',(-1.,0.,0.));
#6373=DIRECTION('',(0.,0.,-1.));
#6374=DIRECTION('',(-1.,0.,0.));
#6375=DIRECTION('',(-1.,0.,0.));
#6376=DIRECTION('',(0.,0.,-1.));
#6377=DIRECTION('',(-1.,0.,0.));
#6378=DIRECTION('',(0.,0.,-1.));
#6379=DIRECTION('',(-1.,0.,0.));
#6380=DIRECTION('',(0.,0.,-1.));
#6381=DIRECTION('',(0.,0.,1.));
#6382=DIRECTION('',(1.,0.,0.));
#6383=DIRECTION('',(0.,0.,-1.));
#6384=DIRECTION('',(0.,0.,-1.));
#6385=DIRECTION('',(-1.,0.,0.));
#6386=DIRECTION('',(0.,0.,1.));
#6387=DIRECTION('',(1.,0.,0.));
#6388=DIRECTION('',(0.,0.,-1.));
#6389=DIRECTION('',(0.,0.,-1.));
#6390=DIRECTION('',(0.,0.,1.));
#6391=DIRECTION('',(1.,0.,0.));
#6392=DIRECTION('',(1.,0.,0.));
#6393=DIRECTION('',(1.,0.,0.));
#6394=DIRECTION('',(0.,-1.,0.));
#6395=DIRECTION('',(1.,0.,0.));
#6396=DIRECTION('',(0.,-1.,0.));
#6397=DIRECTION('',(1.,0.,0.));
#6398=DIRECTION('',(-1.,-1.87350135405495E-16,1.21685779376401E-16));
#6399=DIRECTION('',(1.87350135405495E-16,-1.,3.7148595991706E-16));
#6400=DIRECTION('',(6.86950496486816E-16,-1.,-4.57061403127902E-16));
#6401=DIRECTION('',(-1.,-6.86950496486816E-16,1.21685779376389E-16));
#6402=CARTESIAN_POINT('',(0.,0.,0.));
#6403=CARTESIAN_POINT('',(-0.00413398187534589,0.010314933354332,0.0068072));
#6404=CARTESIAN_POINT('',(-0.0100893114241425,5.20417042793042E-18,0.0068072));
#6405=CARTESIAN_POINT('',(-0.0100893114241425,-1.7347234759768E-18,0.00602678904540461));
#6406=CARTESIAN_POINT('',(-0.0100893114241425,5.20417042793042E-18,0.));
#6407=CARTESIAN_POINT('',(-0.0100893114241426,-4.9274984480842E-17,0.00602678904540501));
#6408=CARTESIAN_POINT('',(-0.00926407226496803,0.00142935615208567,0.00650324109610025));
#6409=CARTESIAN_POINT('',(-0.00842644381484264,0.00288017118556803,0.00680720000000001));
#6410=CARTESIAN_POINT('',(-0.00756698356810691,0.0043688,0.00680720000000001));
#6411=CARTESIAN_POINT('',(-0.00756698356810691,0.0043688,0.0068072));
#6412=CARTESIAN_POINT('',(-0.00756698356810691,0.0043688,0.00680720000000001));
#6413=CARTESIAN_POINT('',(-0.00671073666523493,0.00585186313959776,0.00680720000000001));
#6414=CARTESIAN_POINT('',(-0.00586783431762229,0.00731181283148194,0.00650205143491084));
#6415=CARTESIAN_POINT('',(-0.00504465571207126,0.00873760000000003,0.00602678904540481));
#6416=CARTESIAN_POINT('',(-0.00504465571207127,0.0087376,0.00602678904540461));
#6417=CARTESIAN_POINT('',(-0.00504465571207127,0.0087376,0.0068072));
#6418=CARTESIAN_POINT('',(-0.00504465571207127,0.0087376,0.));
#6419=CARTESIAN_POINT('',(-0.00413398187534589,0.010314933354332,0.));
#6420=CARTESIAN_POINT('',(-0.00413398187534589,-0.010314933354332,0.0068072));
#6421=CARTESIAN_POINT('',(-0.00504465571207127,-0.0087376,0.0068072));
#6422=CARTESIAN_POINT('',(-0.00504465571207127,-0.0087376,0.00602678904540461));
#6423=CARTESIAN_POINT('',(-0.00504465571207127,-0.0087376,0.));
#6424=CARTESIAN_POINT('',(-0.00504465571207124,-0.00873760000000005,0.00602678904540501));
#6425=CARTESIAN_POINT('',(-0.00586989487124578,-0.00730824384791432,0.00650324109610026));
#6426=CARTESIAN_POINT('',(-0.00670752332137117,-0.00585742881443197,0.00680720000000001));
#6427=CARTESIAN_POINT('',(-0.0075669835681069,-0.0043688,0.00680720000000001));
#6428=CARTESIAN_POINT('',(-0.00756698356810691,-0.0043688,0.0068072));
#6429=CARTESIAN_POINT('',(-0.00756698356810691,-0.0043688,0.00680720000000001));
#6430=CARTESIAN_POINT('',(-0.00842323047097888,-0.00288573686040224,0.00680720000000001));
#6431=CARTESIAN_POINT('',(-0.00926613281859153,-0.00142578716851806,0.00650205143491085));
#6432=CARTESIAN_POINT('',(-0.0100893114241426,2.64498759817976E-17,0.00602678904540481));
#6433=CARTESIAN_POINT('',(-0.00413398187534589,-0.010314933354332,0.));
#6434=CARTESIAN_POINT('',(5.61756925238316E-18,-0.0087376,0.0068072));
#6435=CARTESIAN_POINT('',(0.00504465571207128,-0.0087376,0.0068072));
#6436=CARTESIAN_POINT('',(0.00504465571207127,-0.0087376,0.00602678904540461));
#6437=CARTESIAN_POINT('',(0.00504465571207128,-0.0087376,0.));
#6438=CARTESIAN_POINT('',(-2.36129909705544E-19,-0.0087376,0.0068072));
#6439=CARTESIAN_POINT('',(0.00170594066282747,-0.0087376,0.0068072));
#6440=CARTESIAN_POINT('',(0.00341327030332511,-0.0087376,0.00649772944785042));
#6441=CARTESIAN_POINT('',(0.00504465571207127,-0.0087376,0.00602678904540461));
#6442=CARTESIAN_POINT('',(0.,-0.0087376,0.0068072));
#6443=CARTESIAN_POINT('',(-0.00504465571207128,-0.0087376,0.00602678904540464));
#6444=CARTESIAN_POINT('',(-0.00340371094881485,-0.0087376,0.00650048899580034));
#6445=CARTESIAN_POINT('',(-0.0017049277051518,-0.0087376,0.0068072));
#6446=CARTESIAN_POINT('',(1.49859356627126E-18,-0.0087376,0.0068072));
#6447=CARTESIAN_POINT('',(5.61756925238316E-18,-0.0087376,0.));
#6448=CARTESIAN_POINT('',(0.00413398187534589,-0.010314933354332,0.0068072));
#6449=CARTESIAN_POINT('',(0.0100893114241425,3.46944695195361E-18,0.0068072));
#6450=CARTESIAN_POINT('',(0.0100893114241425,0.,0.00602678904540461));
#6451=CARTESIAN_POINT('',(0.0100893114241425,3.46944695195361E-18,0.));
#6452=CARTESIAN_POINT('',(0.0100893114241426,4.73615312627302E-17,0.00602678904540501));
#6453=CARTESIAN_POINT('',(0.00926407226496803,-0.00142935615208568,0.00650324109610025));
#6454=CARTESIAN_POINT('',(0.00842644381484264,-0.00288017118556803,0.00680720000000001));
#6455=CARTESIAN_POINT('',(0.00756698356810691,-0.0043688,0.00680720000000001));
#6456=CARTESIAN_POINT('',(0.00756698356810691,-0.0043688,0.0068072));
#6457=CARTESIAN_POINT('',(0.00756698356810691,-0.0043688,0.00680720000000001));
#6458=CARTESIAN_POINT('',(0.00671073666523493,-0.00585186313959775,0.00680720000000001));
#6459=CARTESIAN_POINT('',(0.00586783431762229,-0.00731181283148194,0.00650205143491084));
#6460=CARTESIAN_POINT('',(0.00504465571207126,-0.00873760000000003,0.00602678904540481));
#6461=CARTESIAN_POINT('',(0.00413398187534589,-0.010314933354332,0.));
#6462=CARTESIAN_POINT('',(0.0109999852608679,-0.00157733335433204,0.0068072));
#6463=CARTESIAN_POINT('',(0.00504465571207127,0.0087376,0.0068072));
#6464=CARTESIAN_POINT('',(0.00504465571207127,0.0087376,0.00602678904540461));
#6465=CARTESIAN_POINT('',(0.00504465571207127,0.0087376,0.));
#6466=CARTESIAN_POINT('',(0.00504465571207124,0.00873760000000004,0.00602678904540501));
#6467=CARTESIAN_POINT('',(0.00586989487124578,0.00730824384791432,0.00650324109610026));
#6468=CARTESIAN_POINT('',(0.00670752332137117,0.00585742881443197,0.00680720000000001));
#6469=CARTESIAN_POINT('',(0.0075669835681069,0.0043688,0.00680720000000001));
#6470=CARTESIAN_POINT('',(0.00756698356810691,0.0043688,0.0068072));
#6471=CARTESIAN_POINT('',(0.0075669835681069,0.0043688,0.00680720000000001));
#6472=CARTESIAN_POINT('',(0.00842323047097888,0.00288573686040224,0.00680720000000001));
#6473=CARTESIAN_POINT('',(0.00926613281859152,0.00142578716851806,0.00650205143491085));
#6474=CARTESIAN_POINT('',(0.0100893114241426,-2.79818636934923E-17,0.00602678904540481));
#6475=CARTESIAN_POINT('',(0.0109999852608679,-0.00157733335433204,0.));
#6476=CARTESIAN_POINT('',(0.,0.0087376,0.0068072));
#6477=CARTESIAN_POINT('',(-0.00504465571207128,0.0087376,0.00602678904540464));
#6478=CARTESIAN_POINT('',(-0.00340371094881485,0.0087376,0.00650048899580034));
#6479=CARTESIAN_POINT('',(-0.0017049277051518,0.0087376,0.0068072));
#6480=CARTESIAN_POINT('',(1.5036505349461E-18,0.0087376,0.0068072));
#6481=CARTESIAN_POINT('',(0.,0.0087376,0.0068072));
#6482=CARTESIAN_POINT('',(-2.3107294103071E-19,0.0087376,0.0068072));
#6483=CARTESIAN_POINT('',(0.00170594066282747,0.0087376,0.0068072));
#6484=CARTESIAN_POINT('',(0.00341327030332511,0.0087376,0.00649772944785042));
#6485=CARTESIAN_POINT('',(0.00504465571207127,0.0087376,0.00602678904540461));
#6486=CARTESIAN_POINT('',(0.,0.0087376,0.));
#6487=CARTESIAN_POINT('',(0.,0.,0.));
#6488=CARTESIAN_POINT('',(0.,0.,0.));
#6489=CARTESIAN_POINT('',(0.0055245,0.,0.));
#6490=CARTESIAN_POINT('',(0.,0.,-0.0381));
#6491=CARTESIAN_POINT('',(0.,0.,-0.0372407404234375));
#6492=CARTESIAN_POINT('',(-0.0047625,0.,-0.0372407404234375));
#6493=CARTESIAN_POINT('',(0.,0.,-0.000762));
#6494=CARTESIAN_POINT('',(0.0047625,0.,-0.000762));
#6495=CARTESIAN_POINT('',(-1.7347234759768E-18,0.,-0.0381));
#6496=CARTESIAN_POINT('',(0.,0.,-0.0381));
#6497=CARTESIAN_POINT('',(-0.0039032404234375,0.,-0.0381));
#6498=CARTESIAN_POINT('',(0.,0.,0.0068072));
#6499=CARTESIAN_POINT('',(0.,0.,0.0068072));
#6500=CARTESIAN_POINT('',(0.,0.,0.0068072));
#6501=CARTESIAN_POINT('',(0.,0.,0.0068072));
#6502=CARTESIAN_POINT('',(0.,0.,0.0068072));
#6503=CARTESIAN_POINT('',(0.,0.,0.0068072));
#6504=CARTESIAN_POINT('',(0.,0.,0.0068072));
#6505=CARTESIAN_POINT('',(0.,0.,0.0068072));
#6506=CARTESIAN_POINT('',(0.,0.,0.0068072));
#6507=CARTESIAN_POINT('',(0.,0.,0.0068072));
#6508=CARTESIAN_POINT('',(0.,0.,0.0068072));
#6509=CARTESIAN_POINT('',(0.,0.,0.0068072));
#6510=CARTESIAN_POINT('',(0.,0.,0.0068072));
#6511=CARTESIAN_POINT('',(0.,0.,-0.000762));
#6512=CARTESIAN_POINT('',(0.,0.,-0.0381));
#6513=CARTESIAN_POINT('',(-0.0897283542354298,-0.135137641711234,-0.204278213710662));
#6514=CARTESIAN_POINT('',(0.,0.09,0.));
#6515=CARTESIAN_POINT('',(0.,0.09,0.));
#6516=CARTESIAN_POINT('',(0.041,0.09,0.));
#6517=CARTESIAN_POINT('',(0.,0.09,0.));
#6518=CARTESIAN_POINT('',(0.,0.09,0.039));
#6519=CARTESIAN_POINT('',(0.,0.,0.));
#6520=CARTESIAN_POINT('',(0.,0.,0.));
#6521=CARTESIAN_POINT('',(0.041,0.,0.));
#6522=CARTESIAN_POINT('',(0.,0.,0.));
#6523=CARTESIAN_POINT('',(0.,0.,0.039));
#6524=CARTESIAN_POINT('',(0.,0.09,0.));
#6525=CARTESIAN_POINT('',(0.,0.09,0.));
#6526=CARTESIAN_POINT('',(-0.0896503542354298,-0.104137641631234,-0.0774361085106635));
#6527=CARTESIAN_POINT('',(0.,0.00131,0.));
#6528=CARTESIAN_POINT('',(0.,-0.00131,0.));
#6529=CARTESIAN_POINT('',(-0.00525,-0.00131,-0.0386450190839648));
#6530=CARTESIAN_POINT('',(0.00525,-0.00131,-0.0386450190839648));
#6531=CARTESIAN_POINT('',(0.00525,0.00131,-0.0386450190839648));
#6532=CARTESIAN_POINT('',(0.00525,0.00131,-0.0386450190839648));
#6533=CARTESIAN_POINT('',(0.,0.00131,0.));
#6534=CARTESIAN_POINT('',(-0.00525,0.00131,-0.0386450190839648));
#6535=CARTESIAN_POINT('',(-0.00525,0.00131,-0.0386450190839648));
#6536=CARTESIAN_POINT('',(0.00525,0.00131,-0.0386450190839648));
#6537=CARTESIAN_POINT('',(0.00525,-0.00131,-0.0386450190839648));
#6538=CARTESIAN_POINT('',(0.00525,-0.00131,-0.0351096496707102));
#6539=CARTESIAN_POINT('',(0.00525,0.00131,-0.0351096496707102));
#6540=CARTESIAN_POINT('',(0.00525,0.00131,-0.0351096496707102));
#6541=CARTESIAN_POINT('',(0.00525,0.00131,-0.0386450190839648));
#6542=CARTESIAN_POINT('',(0.,0.00131,0.));
#6543=CARTESIAN_POINT('',(0.,-0.00131,0.));
#6544=CARTESIAN_POINT('',(-0.00525,-0.00131,-0.0351096496707102));
#6545=CARTESIAN_POINT('',(-0.00525,0.00131,-0.0351096496707102));
#6546=CARTESIAN_POINT('',(-0.00525,0.00131,-0.0351096496707102));
#6547=CARTESIAN_POINT('',(0.,0.00131,0.));
#6548=CARTESIAN_POINT('',(-0.00525,0.00131,-0.0386450190839648));
#6549=CARTESIAN_POINT('',(-0.00525,-0.00131,-0.0386450190839648));
#6550=CARTESIAN_POINT('',(-0.00525,0.00131,-0.0386450190839648));
#6551=CARTESIAN_POINT('',(0.,0.00131,0.));
#6552=CARTESIAN_POINT('',(0.,-0.00131,0.));
#6553=CARTESIAN_POINT('',(-0.0896503542354298,-0.104137641631234,0.00107389162933641));
#6554=CARTESIAN_POINT('',(6.93889390390723E-18,-0.01000000007,-0.03408));
#6555=CARTESIAN_POINT('',(0.00946663159093614,-0.0139561679473873,-0.0278767736634555));
#6556=CARTESIAN_POINT('',(0.0102666200478305,-0.0100000565954907,-0.0275752828436828));
#6557=CARTESIAN_POINT('',(0.00946688821774168,-0.00604360609065003,-0.0278767285229424));
#6558=CARTESIAN_POINT('',(0.00725035830735357,-0.00274839440570845,-0.0285683176118653));
#6559=CARTESIAN_POINT('',(0.00395507415494214,-0.00053339877994205,-0.0292396064107534));
#6560=CARTESIAN_POINT('',(8.7295912523717E-6,0.000265578825293647,-0.0295203456594297));
#6561=CARTESIAN_POINT('',(-0.00395003344396799,-0.000528930247298576,-0.0292410106298082));
#6562=CARTESIAN_POINT('',(-0.00725619049089152,-0.00275303181564925,-0.0285668891854122));
#6563=CARTESIAN_POINT('',(-0.00946785242770053,-0.00604878322242755,-0.0278762714324907));
#6564=CARTESIAN_POINT('',(-0.010265338281535,-0.00999489822950936,-0.0275757620013937));
#6565=CARTESIAN_POINT('',(-0.00947078950931377,-0.0139472845698404,-0.0278753159068785));
#6566=CARTESIAN_POINT('',(-0.00725435049491199,-0.0172490827823861,-0.0285674371250356));
#6567=CARTESIAN_POINT('',(-0.00395206613480992,-0.0194689363159613,-0.0292403663038441));
#6568=CARTESIAN_POINT('',(-3.96206978751156E-7,-0.0202655823062788,-0.029520344557746));
#6569=CARTESIAN_POINT('',(0.00395294398365647,-0.0194687348747586,-0.0292402596637565));
#6570=CARTESIAN_POINT('',(0.00725259756702223,-0.0172494862997466,-0.0285677364036141));
#6571=CARTESIAN_POINT('',(0.00946663159093614,-0.0139561679473873,-0.0278767736634555));
#6572=CARTESIAN_POINT('',(0.0102666200478305,-0.0100000565954907,-0.0275752828436828));
#6573=CARTESIAN_POINT('',(0.00946688821774168,-0.00604360609065003,-0.0278767285229424));
#6574=CARTESIAN_POINT('',(0.01,-0.01000000007,-0.0276757722601882));
#6575=CARTESIAN_POINT('',(6.93889390390723E-18,-0.01000000007,-0.034078));
#6576=CARTESIAN_POINT('',(0.01,-0.01000000007,-0.034078));
#6577=CARTESIAN_POINT('',(0.,-0.0569016393442623,0.));
#6578=CARTESIAN_POINT('',(-0.0132533893149118,-0.00446383140324631,-0.0364099611309221));
#6579=CARTESIAN_POINT('',(-0.0143737540409632,-0.00999787707861307,-0.0359566639800123));
#6580=CARTESIAN_POINT('',(-0.0132515945212353,-0.0155446607023014,-0.0364107901432995));
#6581=CARTESIAN_POINT('',(-0.0101500584303514,-0.0201510160446614,-0.0374462176304152));
#6582=CARTESIAN_POINT('',(-0.00554229810874566,-0.0232510882909091,-0.0384472488580326));
#6583=CARTESIAN_POINT('',(-1.26629420446097E-5,-0.0243729960180894,-0.0388663870917174));
#6584=CARTESIAN_POINT('',(0.00553690033500876,-0.023256909357022,-0.0384491960150612));
#6585=CARTESIAN_POINT('',(0.0101593273036987,-0.0201434215672515,-0.0374437158522921));
#6586=CARTESIAN_POINT('',(0.0132531589529878,-0.0155359599646523,-0.0364100584582362));
#6587=CARTESIAN_POINT('',(0.0143721784014614,-0.0100067959764106,-0.0359571541294907));
#6588=CARTESIAN_POINT('',(0.0132581215780687,-0.00446824126569558,-0.0364087344913512));
#6589=CARTESIAN_POINT('',(0.010666489619777,-0.00061724692514208,-0.0372730694062662));
#6590=CARTESIAN_POINT('',(0.00785058238386626,0.00169977372296183,-0.0379469071648758));
#6591=CARTESIAN_POINT('',(0.00541380149881201,0.00300821979624252,-0.0383754503653669));
#6592=CARTESIAN_POINT('',(0.00278404945627228,0.0038132451617009,-0.0386587997617237));
#6593=CARTESIAN_POINT('',(-0.000935274336576486,0.00418676378220625,-0.0387958699540579));
#6594=CARTESIAN_POINT('',(-0.00553839643887497,0.00325289608103151,-0.0384481705128959));
#6595=CARTESIAN_POINT('',(-0.0101574153340434,0.000145854240069477,-0.0374443881689455));
#6596=CARTESIAN_POINT('',(-0.0132533893149118,-0.00446383140324631,-0.0364099611309221));
#6597=CARTESIAN_POINT('',(-0.0143737540409632,-0.00999787707861307,-0.0359566639800123));
#6598=CARTESIAN_POINT('',(-0.0132515945212353,-0.0155446607023014,-0.0364107901432995));
#6599=CARTESIAN_POINT('',(-0.014,-0.01000000007,-0.0361079011990451));
#6600=CARTESIAN_POINT('',(-1.30606535733962E-17,0.01449999993,0.));
#6601=CARTESIAN_POINT('',(0.038727,0.01449999993,0.));
#6602=CARTESIAN_POINT('',(-2.35994359237075E-18,-0.04400000007,0.));
#6603=CARTESIAN_POINT('',(0.038727,-0.04400000007,0.));
#6604=CARTESIAN_POINT('',(-0.0132533893149118,-0.00446383140324631,0.0364099611309221));
#6605=CARTESIAN_POINT('',(-0.0143737540409632,-0.00999787707861307,0.0359566639800123));
#6606=CARTESIAN_POINT('',(-0.0132515945212353,-0.0155446607023014,0.0364107901432995));
#6607=CARTESIAN_POINT('',(-0.0101500584303514,-0.0201510160446614,0.0374462176304152));
#6608=CARTESIAN_POINT('',(-0.00554229810874566,-0.0232510882909091,0.0384472488580326));
#6609=CARTESIAN_POINT('',(-1.26629420446097E-5,-0.0243729960180894,0.0388663870917174));
#6610=CARTESIAN_POINT('',(0.00553690033500876,-0.023256909357022,0.0384491960150612));
#6611=CARTESIAN_POINT('',(0.0101593273036987,-0.0201434215672515,0.0374437158522921));
#6612=CARTESIAN_POINT('',(0.0132531589529878,-0.0155359599646523,0.0364100584582362));
#6613=CARTESIAN_POINT('',(0.0143721784014614,-0.0100067959764106,0.0359571541294907));
#6614=CARTESIAN_POINT('',(0.0132581215780687,-0.00446824126569558,0.0364087344913512));
#6615=CARTESIAN_POINT('',(0.010666489619777,-0.00061724692514208,0.0372730694062662));
#6616=CARTESIAN_POINT('',(0.00785058238386626,0.00169977372296183,0.0379469071648758));
#6617=CARTESIAN_POINT('',(0.00541380149881201,0.00300821979624252,0.0383754503653669));
#6618=CARTESIAN_POINT('',(0.00278404945627228,0.0038132451617009,0.0386587997617237));
#6619=CARTESIAN_POINT('',(-0.000935274336576486,0.00418676378220625,0.0387958699540579));
#6620=CARTESIAN_POINT('',(-0.00553839643887497,0.00325289608103151,0.0384481705128959));
#6621=CARTESIAN_POINT('',(-0.0101574153340434,0.000145854240069477,0.0374443881689455));
#6622=CARTESIAN_POINT('',(-0.0132533893149118,-0.00446383140324631,0.0364099611309221));
#6623=CARTESIAN_POINT('',(-0.0143737540409632,-0.00999787707861307,0.0359566639800123));
#6624=CARTESIAN_POINT('',(-0.0132515945212353,-0.0155446607023014,0.0364107901432995));
#6625=CARTESIAN_POINT('',(-0.014,-0.01000000007,0.0361079011990451));
#6626=CARTESIAN_POINT('',(0.,-0.0569016393442623,0.));
#6627=CARTESIAN_POINT('',(-2.35994359237075E-18,-0.04400000007,0.));
#6628=CARTESIAN_POINT('',(0.0294270007,-0.04400000007,0.));
#6629=CARTESIAN_POINT('',(0.00946663159093613,-0.00604383219261268,0.0278767736634555));
#6630=CARTESIAN_POINT('',(0.0102666200478305,-0.00999994354450934,0.0275752828436828));
#6631=CARTESIAN_POINT('',(0.00946688821774168,-0.01395639404935,0.0278767285229424));
#6632=CARTESIAN_POINT('',(0.00725035830735357,-0.0172516057342916,0.0285683176118653));
#6633=CARTESIAN_POINT('',(0.00395507415494213,-0.019466601360058,0.0292396064107534));
#6634=CARTESIAN_POINT('',(8.72959125237468E-6,-0.0202655789652937,0.0295203456594297));
#6635=CARTESIAN_POINT('',(-0.00395003344396804,-0.0194710698927014,0.0292410106298082));
#6636=CARTESIAN_POINT('',(-0.0072561904908915,-0.0172469683243508,0.0285668891854122));
#6637=CARTESIAN_POINT('',(-0.00946785242770053,-0.0139512169175724,0.0278762714324907));
#6638=CARTESIAN_POINT('',(-0.010265338281535,-0.0100051019104906,0.0275757620013937));
#6639=CARTESIAN_POINT('',(-0.00947078950931378,-0.00605271557015959,0.0278753159068785));
#6640=CARTESIAN_POINT('',(-0.00725435049491192,-0.00275091735761384,0.0285674371250356));
#6641=CARTESIAN_POINT('',(-0.00395206613480994,-0.000531063824038759,0.0292403663038441));
#6642=CARTESIAN_POINT('',(-3.96206978744596E-7,0.000265582166278759,0.029520344557746));
#6643=CARTESIAN_POINT('',(0.00395294398365648,-0.000531265265241394,0.0292402596637565));
#6644=CARTESIAN_POINT('',(0.00725259756702223,-0.00275051384025345,0.0285677364036141));
#6645=CARTESIAN_POINT('',(0.00946663159093613,-0.00604383219261268,0.0278767736634555));
#6646=CARTESIAN_POINT('',(0.0102666200478305,-0.00999994354450934,0.0275752828436828));
#6647=CARTESIAN_POINT('',(0.00946688821774168,-0.01395639404935,0.0278767285229424));
#6648=CARTESIAN_POINT('',(0.01,-0.01000000007,0.0276757722601882));
#6649=CARTESIAN_POINT('',(-1.70848528828529E-17,0.03650000367,0.));
#6650=CARTESIAN_POINT('',(0.0294270007,0.03650000367,0.));
#6651=CARTESIAN_POINT('',(6.47884089682804E-34,0.04400000007,0.));
#6652=CARTESIAN_POINT('',(-1.84567381193509E-17,0.04400000007,0.));
#6653=CARTESIAN_POINT('',(0.038727,0.04400000007,0.));
#6654=CARTESIAN_POINT('',(0.,-0.0569016393442623,0.));
#6655=CARTESIAN_POINT('',(-1.70299767885476E-17,0.03620000007,0.));
#6656=CARTESIAN_POINT('',(0.038727,0.03620000007,0.));
#6657=CARTESIAN_POINT('',(0.038727,0.03620000007,0.));
#6658=CARTESIAN_POINT('',(-1.70299767885476E-17,0.03620000007,0.));
#6659=CARTESIAN_POINT('',(0.03442700038,0.03620000007,0.));
#6660=CARTESIAN_POINT('',(0.,-0.0569016393442623,0.));
#6661=CARTESIAN_POINT('',(-1.64812224305462E-17,0.03320000007,0.));
#6662=CARTESIAN_POINT('',(0.03442700038,0.03320000007,0.));
#6663=CARTESIAN_POINT('',(0.03442700038,0.03320000007,0.));
#6664=CARTESIAN_POINT('',(-1.64812224305462E-17,0.03320000007,0.));
#6665=CARTESIAN_POINT('',(0.038727,0.03320000007,0.));
#6666=CARTESIAN_POINT('',(0.,-0.0569016393442623,0.));
#6667=CARTESIAN_POINT('',(-1.58958844633116E-17,0.03000000015,0.));
#6668=CARTESIAN_POINT('',(0.038727,0.03000000015,0.));
#6669=CARTESIAN_POINT('',(0.038727,0.03000000015,0.));
#6670=CARTESIAN_POINT('',(-1.58958844633116E-17,0.03000000015,0.));
#6671=CARTESIAN_POINT('',(0.03442700038,0.03000000015,0.));
#6672=CARTESIAN_POINT('',(0.,-0.0569016393442623,0.));
#6673=CARTESIAN_POINT('',(-1.53471301053103E-17,0.02700000015,0.));
#6674=CARTESIAN_POINT('',(0.03442700038,0.02700000015,0.));
#6675=CARTESIAN_POINT('',(0.03442700038,0.02700000015,0.));
#6676=CARTESIAN_POINT('',(-1.53471301053103E-17,0.0270000001499999,0.));
#6677=CARTESIAN_POINT('',(0.038727,0.02700000015,0.));
#6678=CARTESIAN_POINT('',(0.,-0.0569016393442623,0.));
#6679=CARTESIAN_POINT('',(-1.47617921380757E-17,0.02380000023,0.));
#6680=CARTESIAN_POINT('',(0.038727,0.02380000023,0.));
#6681=CARTESIAN_POINT('',(0.038727,0.02380000023,0.));
#6682=CARTESIAN_POINT('',(-1.47617921380757E-17,0.02380000023,0.));
#6683=CARTESIAN_POINT('',(0.03442700038,0.02380000023,0.));
#6684=CARTESIAN_POINT('',(0.,-0.0569016393442623,0.));
#6685=CARTESIAN_POINT('',(-1.42130377800744E-17,0.02080000023,0.));
#6686=CARTESIAN_POINT('',(0.03442700038,0.02080000023,0.));
#6687=CARTESIAN_POINT('',(0.03442700038,0.02080000023,0.));
#6688=CARTESIAN_POINT('',(-1.42130377800744E-17,0.0208000002299999,0.));
#6689=CARTESIAN_POINT('',(0.038727,0.02080000023,0.));
#6690=CARTESIAN_POINT('',(0.,-0.0569016393442623,0.));
#6691=CARTESIAN_POINT('',(-1.36276998128398E-17,0.01760000031,0.));
#6692=CARTESIAN_POINT('',(0.038727,0.01760000031,0.));
#6693=CARTESIAN_POINT('',(0.038727,0.01760000031,0.));
#6694=CARTESIAN_POINT('',(-1.36276998128398E-17,0.01760000031,0.));
#6695=CARTESIAN_POINT('',(0.03442700038,0.01760000031,0.));
#6696=CARTESIAN_POINT('',(0.,-0.0569016393442623,0.));
#6697=CARTESIAN_POINT('',(-1.30606535733962E-17,0.01449999993,0.));
#6698=CARTESIAN_POINT('',(0.03442700038,0.01449999993,0.));
#6699=CARTESIAN_POINT('',(0.03442700038,0.01449999993,0.));
#6700=CARTESIAN_POINT('',(0.038727,-0.04400000007,0.));
#6701=CARTESIAN_POINT('',(0.0294270007,0.03650000367,0.));
#6702=CARTESIAN_POINT('',(6.93889390390723E-18,-0.01000000007,-0.034078));
#6703=CARTESIAN_POINT('',(6.93889390390723E-18,-0.01000000007,-0.034078));
#6704=CARTESIAN_POINT('',(0.014,-0.01000000007,-0.034078));
#6705=CARTESIAN_POINT('',(6.93889390390723E-18,-0.01000000007,-0.034078));
#6706=CARTESIAN_POINT('',(6.93889390390723E-18,-0.01000000007,0.034078));
#6707=CARTESIAN_POINT('',(6.93889390390723E-18,-0.01000000007,0.034078));
#6708=CARTESIAN_POINT('',(0.014,-0.01000000007,0.034078));
#6709=CARTESIAN_POINT('',(6.93889390390723E-18,-0.01000000007,0.034078));
#6710=CARTESIAN_POINT('',(6.93889390390723E-18,-0.01000000007,0.034078));
#6711=CARTESIAN_POINT('',(0.01,-0.01000000007,0.034078));
#6712=CARTESIAN_POINT('',(6.93889390390723E-18,-0.01000000007,-0.03408));
#6713=CARTESIAN_POINT('',(-0.0896503542354298,-0.104137641631234,-0.0334361084406635));
#6714=CARTESIAN_POINT('',(-0.0896503542354298,-0.104137641631234,-0.0176261085106635));
#6715=CARTESIAN_POINT('',(-0.0897283542354298,-0.0731376415512337,-0.204278213710662));
#6716=CARTESIAN_POINT('',(0.,0.,0.034));
#6717=CARTESIAN_POINT('',(0.,0.,0.034));
#6718=CARTESIAN_POINT('',(0.0075,0.,0.034));
#6719=CARTESIAN_POINT('',(0.,6.12323399573677E-19,0.034));
#6720=CARTESIAN_POINT('',(0.01,6.12323399573677E-19,0.034));
#6721=CARTESIAN_POINT('',(0.,0.,-0.034));
#6722=CARTESIAN_POINT('',(0.,0.,-0.034));
#6723=CARTESIAN_POINT('',(0.0075,0.,-0.034));
#6724=CARTESIAN_POINT('',(0.,6.12323399573677E-19,-0.034));
#6725=CARTESIAN_POINT('',(0.01,6.12323399573677E-19,-0.034));
#6726=CARTESIAN_POINT('',(0.,0.,0.034));
#6727=CARTESIAN_POINT('',(0.,6.12323399573677E-19,-0.0747896763833597));
#6728=CARTESIAN_POINT('',(-0.0897283542354298,-0.104137641631234,-0.0434361085106635));
#6729=CARTESIAN_POINT('',(0.,-0.0684221052,-0.0669999996));
#6730=CARTESIAN_POINT('',(0.0196214168703486,-0.0924221052,-0.0669999996));
#6731=CARTESIAN_POINT('',(0.0196214168703486,-0.0924221052,-0.0100000004));
#6732=CARTESIAN_POINT('',(0.0196214168703486,-0.0924221052,0.0100000004));
#6733=CARTESIAN_POINT('',(0.,-0.0684221052,0.0100000004));
#6734=CARTESIAN_POINT('',(-0.0196214168703486,-0.0924221052,0.0100000004));
#6735=CARTESIAN_POINT('',(-0.0196214168703486,-0.0924221052,-0.0669999996));
#6736=CARTESIAN_POINT('',(-0.0196214168703486,-0.0924221052,-0.0100000004));
#6737=CARTESIAN_POINT('',(0.,-0.0684221052,-0.0100000004));
#6738=CARTESIAN_POINT('',(0.,-0.0684221052,-0.0100000004));
#6739=CARTESIAN_POINT('',(-0.0196214168703486,-0.0924221052,-0.0100000004));
#6740=CARTESIAN_POINT('',(-0.0196214168703486,-0.0924221052,-0.0102726071240878));
#6741=CARTESIAN_POINT('',(-0.0195383172075569,-0.0921885784050125,-0.0107990864640417));
#6742=CARTESIAN_POINT('',(-0.0193531124817403,-0.0916745903152378,-0.0110000004));
#6743=CARTESIAN_POINT('',(-0.0192613602842582,-0.0914221052,-0.0110000004));
#6744=CARTESIAN_POINT('',(-0.0192613602842583,-0.0914221052,-0.0110000004));
#6745=CARTESIAN_POINT('',(0.,-0.0684221052,-0.0110000004));
#6746=CARTESIAN_POINT('',(0.0192613602842582,-0.0914221052,-0.0110000004));
#6747=CARTESIAN_POINT('',(0.0196214168703486,-0.0924221052,-0.0100000004));
#6748=CARTESIAN_POINT('',(0.0196214168703486,-0.0924221052,-0.0102726071240878));
#6749=CARTESIAN_POINT('',(0.0195383172075569,-0.0921885784050125,-0.0107990864640417));
#6750=CARTESIAN_POINT('',(0.0193531124817403,-0.0916745903152378,-0.0110000004));
#6751=CARTESIAN_POINT('',(0.0192613602842582,-0.0914221052,-0.0110000004));
#6752=CARTESIAN_POINT('',(0.,-0.0684221052,0.0100000004));
#6753=CARTESIAN_POINT('',(-0.0196214168703486,-0.0924221052,0.0100000004));
#6754=CARTESIAN_POINT('',(-0.0196214168703486,-0.0924221052,0.0102726071240878));
#6755=CARTESIAN_POINT('',(-0.0195383172075741,-0.0921885784050062,0.0107990864640417));
#6756=CARTESIAN_POINT('',(-0.0193531124817059,-0.0916745903152503,0.0110000004));
#6757=CARTESIAN_POINT('',(-0.0192613602842582,-0.0914221052,0.0110000004));
#6758=CARTESIAN_POINT('',(-0.0192613602842582,-0.0914221052,0.0110000004));
#6759=CARTESIAN_POINT('',(0.0196214168703486,-0.0924221052,0.0100000004));
#6760=CARTESIAN_POINT('',(0.0196214168703486,-0.0924221052,0.0102726071240878));
#6761=CARTESIAN_POINT('',(0.0195383172075741,-0.0921885784050062,0.0107990864640417));
#6762=CARTESIAN_POINT('',(0.0193531124817059,-0.0916745903152503,0.0110000004));
#6763=CARTESIAN_POINT('',(0.0192613602842582,-0.0914221052,0.0110000004));
#6764=CARTESIAN_POINT('',(0.0192613602842582,-0.0914221052,0.0110000004));
#6765=CARTESIAN_POINT('',(0.,-0.0684221052,0.0110000004));
#6766=CARTESIAN_POINT('',(-0.0196214168703486,-0.0914221052,-0.0100000004));
#6767=CARTESIAN_POINT('',(-0.03550000008,-0.0914221052,-0.0100000004));
#6768=CARTESIAN_POINT('',(-0.03650000008,-0.0924221052,-0.0100000004));
#6769=CARTESIAN_POINT('',(-0.03550000008,-0.0914221052,-0.0110000004));
#6770=CARTESIAN_POINT('',(-0.03650000008,-0.0914221052,-0.0110000004));
#6771=CARTESIAN_POINT('',(-0.0196214168703486,-0.0924221052,-0.0100000004));
#6772=CARTESIAN_POINT('',(-0.0196214168703486,-0.0914221052,0.0100000004));
#6773=CARTESIAN_POINT('',(-0.03550000008,-0.0914221052,0.0100000004));
#6774=CARTESIAN_POINT('',(-0.03550000008,-0.0914221052,0.0110000004));
#6775=CARTESIAN_POINT('',(-0.03650000008,-0.0924221052,0.0100000004));
#6776=CARTESIAN_POINT('',(-0.0196214168703486,-0.0924221052,0.0100000004));
#6777=CARTESIAN_POINT('',(0.03650000008,-0.0914221051999999,0.0110000004));
#6778=CARTESIAN_POINT('',(0.0469715027961281,-0.0914221052,-0.0100000004));
#6779=CARTESIAN_POINT('',(0.0196214168703486,-0.0914221052,-0.0110000004));
#6780=CARTESIAN_POINT('',(0.03550000008,-0.0914221052,-0.0110000004));
#6781=CARTESIAN_POINT('',(0.03550000008,-0.0914221052,-0.0100000004));
#6782=CARTESIAN_POINT('',(0.03650000008,-0.0924221052,-0.0100000004));
#6783=CARTESIAN_POINT('',(0.03650000008,-0.0924221052,-0.0100000004));
#6784=CARTESIAN_POINT('',(0.0469715027961281,-0.0914221052,0.0100000004));
#6785=CARTESIAN_POINT('',(0.0469715027961281,-0.0924221052,0.0100000004));
#6786=CARTESIAN_POINT('',(0.03650000008,-0.0924221052,0.0100000004));
#6787=CARTESIAN_POINT('',(0.03550000008,-0.0914221052,0.0100000004));
#6788=CARTESIAN_POINT('',(0.03550000008,-0.0914221052,0.0110000004));
#6789=CARTESIAN_POINT('',(0.03650000008,-0.0914221052,0.0110000004));
#6790=CARTESIAN_POINT('',(-0.03550000008,-0.0374221052,0.0100000004));
#6791=CARTESIAN_POINT('',(-0.03550000008,-0.0746532949430514,0.0100000004));
#6792=CARTESIAN_POINT('',(-0.03650000008,-0.0746532949430514,0.0100000004));
#6793=CARTESIAN_POINT('',(-0.03550000008,-0.0746532949430514,0.0110000004));
#6794=CARTESIAN_POINT('',(-0.03650000008,-0.0582659958948477,0.0100000004));
#6795=CARTESIAN_POINT('',(-0.03550000008,-0.0924221052,0.0110000004));
#6796=CARTESIAN_POINT('',(-0.03550000008,1.11917648088112E-18,-0.0100000004));
#6797=CARTESIAN_POINT('',(-0.03550000008,-0.0746532949430514,-0.0100000004));
#6798=CARTESIAN_POINT('',(-0.03550000008,-0.0746532949430514,-0.0110000004));
#6799=CARTESIAN_POINT('',(-0.03650000008,-0.0746532949430514,-0.0100000004));
#6800=CARTESIAN_POINT('',(-0.03550000008,-0.0374221052,-0.0110000004));
#6801=CARTESIAN_POINT('',(-0.03650000008,1.11917648088112E-18,-0.0100000004));
#6802=CARTESIAN_POINT('',(-0.03650000008,0.,0.));
#6803=CARTESIAN_POINT('',(-0.03650000008,-0.0746532949430514,0.));
#6804=CARTESIAN_POINT('',(-0.03650000008,-0.0924221052,0.));
#6805=CARTESIAN_POINT('',(0.,0.,-0.0130000004));
#6806=CARTESIAN_POINT('',(0.,-0.0746532949430514,-0.0130000004));
#6807=CARTESIAN_POINT('',(0.0252422715773777,-0.0746532949430514,-0.0130000004));
#6808=CARTESIAN_POINT('',(0.0231769772486856,-0.0746532949430514,-0.0130000004));
#6809=CARTESIAN_POINT('',(0.,-0.0684221052,-0.0130000004));
#6810=CARTESIAN_POINT('',(-0.0252422715773777,-0.0746532949430514,-0.0130000004));
#6811=CARTESIAN_POINT('',(0.,-0.0746532949430514,-0.0130000004));
#6812=CARTESIAN_POINT('',(-0.0231769772486856,-0.0746532949430514,-0.0130000004));
#6813=CARTESIAN_POINT('',(0.,-0.0684221052,-0.0130000004));
#6814=CARTESIAN_POINT('',(0.,-0.0684221052,-0.0120000004));
#6815=CARTESIAN_POINT('',(0.,-0.0684221052,-0.0110000004));
#6816=CARTESIAN_POINT('',(-0.0262711300553686,-0.0746532949430514,-0.0110000004));
#6817=CARTESIAN_POINT('',(0.0262711300553686,-0.0746532949430514,-0.0110000004));
#6818=CARTESIAN_POINT('',(-0.0262711300553686,-0.0746532949430514,-0.0110000004));
#6819=CARTESIAN_POINT('',(-0.0260041493105404,-0.0746532949430514,-0.0110000004));
#6820=CARTESIAN_POINT('',(-0.0254743722652179,-0.0746532949430514,-0.011208704207599));
#6821=CARTESIAN_POINT('',(-0.0252422715773777,-0.0746532949430514,-0.0117351103746111));
#6822=CARTESIAN_POINT('',(-0.0252422715773777,-0.0746532949430514,-0.0120000004));
#6823=CARTESIAN_POINT('',(-0.0252422715773777,-0.0746532949430514,-0.0120000004));
#6824=CARTESIAN_POINT('',(0.,-0.0684221052,-0.0120000004));
#6825=CARTESIAN_POINT('',(0.0252422715773777,-0.0746532949430514,-0.0120000004));
#6826=CARTESIAN_POINT('',(0.0252422715773777,-0.0746532949430514,-0.0120000004));
#6827=CARTESIAN_POINT('',(0.0252422715773777,-0.0746532949430514,-0.0117324512139406));
#6828=CARTESIAN_POINT('',(0.0254742124828446,-0.0746532949430514,-0.0112095401021891));
#6829=CARTESIAN_POINT('',(0.0260054993852186,-0.0746532949430514,-0.0110000004));
#6830=CARTESIAN_POINT('',(0.0262711300553686,-0.0746532949430514,-0.0110000004));
#6831=CARTESIAN_POINT('',(0.,-0.0684221052,-0.0130000004));
#6832=CARTESIAN_POINT('',(0.0252422715773777,-0.0746532949430514,-0.0130000004));
#6833=CARTESIAN_POINT('',(-0.0252422715773777,-0.0746532949430514,-0.0130000004));
#6834=CARTESIAN_POINT('',(0.,-0.0684221052,0.0120000004));
#6835=CARTESIAN_POINT('',(0.,-0.0684221052,0.0120000004));
#6836=CARTESIAN_POINT('',(-0.0252422715773777,-0.0746532949430514,0.0120000004));
#6837=CARTESIAN_POINT('',(0.0252422715773777,-0.0746532949430514,0.0120000004));
#6838=CARTESIAN_POINT('',(-0.0252422715773777,-0.0746532949430514,0.0120000004));
#6839=CARTESIAN_POINT('',(-0.0252422715773777,-0.0746532949430514,0.0117340892011008));
#6840=CARTESIAN_POINT('',(-0.0254741318712697,-0.0746532949430514,0.0112081301589468));
#6841=CARTESIAN_POINT('',(-0.0260068950976863,-0.0746532949430514,0.0110000004));
#6842=CARTESIAN_POINT('',(-0.0262711300553686,-0.0746532949430514,0.0110000004));
#6843=CARTESIAN_POINT('',(-0.0262711300553686,-0.0746532949430514,0.0110000004));
#6844=CARTESIAN_POINT('',(0.,-0.0684221052,0.0110000004));
#6845=CARTESIAN_POINT('',(0.0262711300553686,-0.0746532949430514,0.0110000004));
#6846=CARTESIAN_POINT('',(0.0262711300553686,-0.0746532949430514,0.0110000004));
#6847=CARTESIAN_POINT('',(0.0260068432764003,-0.0746532949430514,0.0110000004));
#6848=CARTESIAN_POINT('',(0.0254746601402995,-0.0746532949430514,0.0112068289794583));
#6849=CARTESIAN_POINT('',(0.0252422715773777,-0.0746532949430514,0.0117357303784197));
#6850=CARTESIAN_POINT('',(0.0252422715773777,-0.0746532949430514,0.0120000004));
#6851=CARTESIAN_POINT('',(0.,0.,0.0130000004));
#6852=CARTESIAN_POINT('',(0.,-0.0746532949430514,0.0130000004));
#6853=CARTESIAN_POINT('',(-0.0252422715773777,-0.0746532949430514,0.0130000004));
#6854=CARTESIAN_POINT('',(-0.0231769772486856,-0.0746532949430514,0.0130000004));
#6855=CARTESIAN_POINT('',(0.,-0.0684221052,0.0130000004));
#6856=CARTESIAN_POINT('',(0.0252422715773777,-0.0746532949430514,0.0130000004));
#6857=CARTESIAN_POINT('',(0.,-0.0746532949430514,0.0130000004));
#6858=CARTESIAN_POINT('',(0.0231769772486856,-0.0746532949430514,0.0130000004));
#6859=CARTESIAN_POINT('',(0.,-0.0684221052,0.0130000004));
#6860=CARTESIAN_POINT('',(0.,-0.0684221052,0.0130000004));
#6861=CARTESIAN_POINT('',(-0.0252422715773777,-0.0746532949430514,0.0130000004));
#6862=CARTESIAN_POINT('',(0.0252422715773777,-0.0746532949430514,0.0130000004));
#6863=CARTESIAN_POINT('',(0.,-0.0684221052,-0.01200000032));
#6864=CARTESIAN_POINT('',(0.0231769772486856,-0.0746532949430514,-0.01200000032));
#6865=CARTESIAN_POINT('',(-0.0231769772486856,-0.0746532949430514,-0.01200000032));
#6866=CARTESIAN_POINT('',(0.03550000008,-1.11917648088113E-18,0.0100000004));
#6867=CARTESIAN_POINT('',(0.03550000008,-0.0746532949430514,0.0100000004));
#6868=CARTESIAN_POINT('',(0.03550000008,-0.0746532949430514,0.0110000004));
#6869=CARTESIAN_POINT('',(0.03650000008,-0.0746532949430514,0.0100000004));
#6870=CARTESIAN_POINT('',(0.03550000008,-0.0374221052,0.0110000004));
#6871=CARTESIAN_POINT('',(0.03650000008,-1.11917648088113E-18,0.0100000004));
#6872=CARTESIAN_POINT('',(0.03550000008,-0.0374221052,-0.0100000004));
#6873=CARTESIAN_POINT('',(0.03550000008,-0.0746532949430514,-0.0100000004));
#6874=CARTESIAN_POINT('',(0.03650000008,-0.0746532949430514,-0.0100000004));
#6875=CARTESIAN_POINT('',(0.03550000008,-0.0746532949430514,-0.0110000004));
#6876=CARTESIAN_POINT('',(0.03650000008,-0.0582659958948477,-0.0100000004));
#6877=CARTESIAN_POINT('',(0.03550000008,-0.0924221052,-0.0110000004));
#6878=CARTESIAN_POINT('',(0.03650000008,0.,0.));
#6879=CARTESIAN_POINT('',(0.03650000008,-0.0746532949430514,0.));
#6880=CARTESIAN_POINT('',(0.03650000008,-0.0924221052,0.));
#6881=CARTESIAN_POINT('',(0.03650000008,-0.0374221052,0.0110000004));
#6882=CARTESIAN_POINT('',(0.03650000008,-0.0746532949430514,0.0110000004));
#6883=CARTESIAN_POINT('',(0.03650000008,-0.0746532949430514,0.0110000004));
#6884=CARTESIAN_POINT('',(0.03650000008,-0.0374221052,-0.0110000004));
#6885=CARTESIAN_POINT('',(0.03650000008,-0.0746532949430514,-0.0110000004));
#6886=CARTESIAN_POINT('',(0.03650000008,-0.0746532949430514,-0.0110000004));
#6887=CARTESIAN_POINT('',(-0.0196214168703486,-0.0924221052,-0.0669999996));
#6888=CARTESIAN_POINT('',(-0.03100000008,-0.0924221052,0.));
#6889=CARTESIAN_POINT('',(-0.03550000008,-0.0924221052,0.));
#6890=CARTESIAN_POINT('',(-0.03100000008,0.,0.));
#6891=CARTESIAN_POINT('',(-0.03100000008,-0.0746532949430514,0.));
#6892=CARTESIAN_POINT('',(-0.03100000008,-0.0746532949430514,-0.0045));
#6893=CARTESIAN_POINT('',(0.0469715027961281,-0.0924221052,-0.0669999996));
#6894=CARTESIAN_POINT('',(0.03100000008,-0.0924221052,0.));
#6895=CARTESIAN_POINT('',(0.03100000008,-0.0924221052,0.0045));
#6896=CARTESIAN_POINT('',(0.03100000008,0.,0.));
#6897=CARTESIAN_POINT('',(0.03100000008,-0.0746532949430514,0.));
#6898=CARTESIAN_POINT('',(0.03100000008,-0.0746532949430514,-0.0045));
#6899=CARTESIAN_POINT('',(0.0434268042445183,-0.0746532949430514,0.0110000004));
#6900=CARTESIAN_POINT('',(0.0434268042445183,-0.0746532949430514,0.0110000004));
#6901=CARTESIAN_POINT('',(-0.0897283542354298,-0.104137641631234,-0.111856108510662));
#6902=CARTESIAN_POINT('',(-0.0896503542354298,-0.104137641631234,-0.0113261082106636));
#6903=CARTESIAN_POINT('',(0.03650000008,-0.0374221052,-0.0110000004));
#6904=CARTESIAN_POINT('',(0.03550000008,-0.0924221052,-0.0110000004));
#6905=CARTESIAN_POINT('',(0.03550000008,-0.0578844846861027,-0.0110000004));
#6906=CARTESIAN_POINT('',(0.03550000008,-0.0746532949430514,-0.0110000004));
#6907=CARTESIAN_POINT('',(0.03650000008,-0.0746532949430514,-0.0110000004));
#6908=CARTESIAN_POINT('',(0.0262711300553686,-0.0746532949430514,-0.0110000004));
#6909=CARTESIAN_POINT('',(0.,-0.0684221052,-0.0110000004));
#6910=CARTESIAN_POINT('',(-0.0262711300553686,-0.0746532949430514,-0.0110000004));
#6911=CARTESIAN_POINT('',(0.03650000008,-0.0746532949430514,-0.0110000004));
#6912=CARTESIAN_POINT('',(-0.03550000008,-0.0746532949430514,-0.0110000004));
#6913=CARTESIAN_POINT('',(-0.03550000008,-0.0374221052,-0.0110000004));
#6914=CARTESIAN_POINT('',(-0.03550000008,-0.0578844846861027,-0.0110000004));
#6915=CARTESIAN_POINT('',(-0.0479406149651572,-0.0267770382679513,-0.0110000004));
#6916=CARTESIAN_POINT('',(-0.0200162970866487,-0.0452885101813074,-0.0110000004));
#6917=CARTESIAN_POINT('',(0.,-0.0684221052,-0.0110000004));
#6918=CARTESIAN_POINT('',(0.0200162970866487,-0.0452885101813074,-0.0110000004));
#6919=CARTESIAN_POINT('',(0.0479406149651572,-0.0267770382679513,-0.0110000004));
#6920=CARTESIAN_POINT('',(0.03650000008,-0.0374221052,0.0110000004));
#6921=CARTESIAN_POINT('',(0.03650000008,-0.0746532949430514,0.0110000004));
#6922=CARTESIAN_POINT('',(0.03550000008,-0.0746532949430514,0.0110000004));
#6923=CARTESIAN_POINT('',(0.0262711300553686,-0.0746532949430514,0.0110000004));
#6924=CARTESIAN_POINT('',(0.03550000008,-0.0374221052,0.0110000004));
#6925=CARTESIAN_POINT('',(0.03550000008,-0.0578844846861027,0.0110000004));
#6926=CARTESIAN_POINT('',(0.0479406149651572,-0.0267770382679513,0.0110000004));
#6927=CARTESIAN_POINT('',(0.0200162970866487,-0.0452885101813074,0.0110000004));
#6928=CARTESIAN_POINT('',(0.,-0.0684221052,0.0110000004));
#6929=CARTESIAN_POINT('',(-0.0200162970866487,-0.0452885101813074,0.0110000004));
#6930=CARTESIAN_POINT('',(-0.0479406149651572,-0.0267770382679513,0.0110000004));
#6931=CARTESIAN_POINT('',(-0.03550000008,-0.0578844846861027,0.0110000004));
#6932=CARTESIAN_POINT('',(-0.03550000008,-0.0924221052,0.0110000004));
#6933=CARTESIAN_POINT('',(-0.03550000008,-0.0746532949430514,0.0110000004));
#6934=CARTESIAN_POINT('',(0.03650000008,-0.0746532949430514,0.0110000004));
#6935=CARTESIAN_POINT('',(-0.0262711300553686,-0.0746532949430514,0.0110000004));
#6936=CARTESIAN_POINT('',(0.,-0.0684221052,0.0110000004));
#6937=CARTESIAN_POINT('',(0.03650000008,0.,0.));
#6938=CARTESIAN_POINT('',(0.03650000008,-0.0746532949430514,0.));
#6939=CARTESIAN_POINT('',(0.03650000008,-0.0746532949430514,-0.0100000004));
#6940=CARTESIAN_POINT('',(0.03650000008,-0.0746532949430514,0.0100000004));
#6941=CARTESIAN_POINT('',(0.03650000008,-0.0582659958948477,-0.0100000004));
#6942=CARTESIAN_POINT('',(0.03650000008,-0.0578844846861027,-0.0100000004));
#6943=CARTESIAN_POINT('',(0.03650000008,-0.0578844846861027,0.0100000004));
#6944=CARTESIAN_POINT('',(0.03650000008,-0.0578844846861027,0.0100000004));
#6945=CARTESIAN_POINT('',(0.03650000008,-1.11917648088113E-18,0.0100000004));
#6946=CARTESIAN_POINT('',(-0.03650000008,0.,0.));
#6947=CARTESIAN_POINT('',(-0.03650000008,1.11917648088112E-18,-0.0100000004));
#6948=CARTESIAN_POINT('',(-0.03650000008,-0.0578844846861027,-0.0100000004));
#6949=CARTESIAN_POINT('',(-0.03650000008,-0.0746532949430514,-0.0100000004));
#6950=CARTESIAN_POINT('',(-0.03650000008,-0.0746532949430514,0.));
#6951=CARTESIAN_POINT('',(-0.03650000008,-0.0746532949430514,0.0100000004));
#6952=CARTESIAN_POINT('',(-0.03650000008,-0.0582659958948477,0.0100000004));
#6953=CARTESIAN_POINT('',(-0.03650000008,-0.0578844846861027,0.0100000004));
#6954=CARTESIAN_POINT('',(-0.03650000008,-0.0578844846861027,-0.0100000004));
#6955=CARTESIAN_POINT('',(0.,-0.0684221052,-0.01200000032));
#6956=CARTESIAN_POINT('',(0.0231769772486856,-0.0746532949430514,-0.01200000032));
#6957=CARTESIAN_POINT('',(0.0231769772486856,-0.0746532949430514,0.0130000004));
#6958=CARTESIAN_POINT('',(0.0231769772486856,-0.0746532949430514,-0.0130000004));
#6959=CARTESIAN_POINT('',(0.,-0.0684221052,0.0130000004));
#6960=CARTESIAN_POINT('',(-0.0231769772486856,-0.0746532949430514,0.0130000004));
#6961=CARTESIAN_POINT('',(-0.0231769772486856,-0.0746532949430514,-0.01200000032));
#6962=CARTESIAN_POINT('',(-0.0231769772486856,-0.0746532949430514,-0.0130000004));
#6963=CARTESIAN_POINT('',(0.,-0.0684221052,-0.0130000004));
#6964=CARTESIAN_POINT('',(0.03100000008,0.,0.));
#6965=CARTESIAN_POINT('',(0.0293798995199573,-0.0534809425826498,0.00430172818359));
#6966=CARTESIAN_POINT('',(0.0309881374462023,-0.0545317846725483,0.00459986185281222));
#6967=CARTESIAN_POINT('',(0.0326675511752334,-0.0554881302704746,0.00429882440516112));
#6968=CARTESIAN_POINT('',(0.0341979731548129,-0.0562441547182963,0.00334152801974006));
#6969=CARTESIAN_POINT('',(0.0352891605534319,-0.0567197587438045,0.00176416161650936));
#6970=CARTESIAN_POINT('',(0.0356378125150989,-0.0568608009129647,-0.000181591276415526));
#6971=CARTESIAN_POINT('',(0.0351390741350192,-0.0566574377320471,-0.00209014083998486));
#6972=CARTESIAN_POINT('',(0.0339352100276026,-0.0561220403071199,-0.00357295922054393));
#6973=CARTESIAN_POINT('',(0.0323479956911139,-0.0553167615665181,-0.00440742187852888));
#6974=CARTESIAN_POINT('',(0.0306663015201423,-0.0543326379667634,-0.00458696466905457));
#6975=CARTESIAN_POINT('',(0.029082531685936,-0.0532708711617687,-0.0041774832675469));
#6976=CARTESIAN_POINT('',(0.027722072208117,-0.0522417406979562,-0.0032332420396007));
#6977=CARTESIAN_POINT('',(0.0267179667732945,-0.0514002809467995,-0.00175955242131977));
#6978=CARTESIAN_POINT('',(0.0263582399151791,-0.0510791744710138,0.000191439326551355));
#6979=CARTESIAN_POINT('',(0.0268710273639056,-0.0515336505560397,0.00208237089075824));
#6980=CARTESIAN_POINT('',(0.0279584485193938,-0.0524292452239578,0.0034539923091798));
#6981=CARTESIAN_POINT('',(0.0293798995199573,-0.0534809425826498,0.00430172818359));
#6982=CARTESIAN_POINT('',(0.0309881374462023,-0.0545317846725483,0.00459986185281222));
#6983=CARTESIAN_POINT('',(0.0326675511752334,-0.0554881302704746,0.00429882440516112));
#6984=CARTESIAN_POINT('',(0.03100000008,-0.0545160352572196,0.0045));
#6985=CARTESIAN_POINT('',(0.03100000008,-0.0746532949430514,0.));
#6986=CARTESIAN_POINT('',(0.03100000008,-0.0746532949430514,-0.0045));
#6987=CARTESIAN_POINT('',(-0.03100000008,0.,0.));
#6988=CARTESIAN_POINT('',(-0.0293798995199573,-0.0534809425826498,0.00430172818359));
#6989=CARTESIAN_POINT('',(-0.0309881374462023,-0.0545317846725483,0.00459986185281222));
#6990=CARTESIAN_POINT('',(-0.0326675511752334,-0.0554881302704746,0.00429882440516112));
#6991=CARTESIAN_POINT('',(-0.0341979731548129,-0.0562441547182964,0.00334152801974006));
#6992=CARTESIAN_POINT('',(-0.0352891605534319,-0.0567197587438045,0.00176416161650936));
#6993=CARTESIAN_POINT('',(-0.0356378125150989,-0.0568608009129647,-0.000181591276415529));
#6994=CARTESIAN_POINT('',(-0.0351390741350192,-0.0566574377320471,-0.00209014083998489));
#6995=CARTESIAN_POINT('',(-0.0339352100276026,-0.0561220403071199,-0.00357295922054392));
#6996=CARTESIAN_POINT('',(-0.0323479956911138,-0.0553167615665181,-0.00440742187852889));
#6997=CARTESIAN_POINT('',(-0.0306663015201423,-0.0543326379667634,-0.00458696466905456));
#6998=CARTESIAN_POINT('',(-0.029082531685936,-0.0532708711617687,-0.00417748326754691));
#6999=CARTESIAN_POINT('',(-0.0277220722081169,-0.0522417406979561,-0.00323324203960068));
#7000=CARTESIAN_POINT('',(-0.0267179667732945,-0.0514002809467995,-0.00175955242131978));
#7001=CARTESIAN_POINT('',(-0.0263582399151791,-0.0510791744710138,0.000191439326551348));
#7002=CARTESIAN_POINT('',(-0.0268710273639056,-0.0515336505560397,0.00208237089075823));
#7003=CARTESIAN_POINT('',(-0.0279584485193938,-0.0524292452239578,0.00345399230917982));
#7004=CARTESIAN_POINT('',(-0.0293798995199573,-0.0534809425826498,0.00430172818359));
#7005=CARTESIAN_POINT('',(-0.0309881374462023,-0.0545317846725483,0.00459986185281222));
#7006=CARTESIAN_POINT('',(-0.0326675511752334,-0.0554881302704746,0.00429882440516112));
#7007=CARTESIAN_POINT('',(-0.03100000008,-0.0545160352572196,0.0045));
#7008=CARTESIAN_POINT('',(-0.03100000008,-0.0746532949430514,0.));
#7009=CARTESIAN_POINT('',(-0.03100000008,-0.0746532949430514,-0.0045));
#7010=CARTESIAN_POINT('',(0.,-0.0684221052,0.0130000004));
#7011=CARTESIAN_POINT('',(-0.0252422715773777,-0.0746532949430514,0.0130000004));
#7012=CARTESIAN_POINT('',(-0.0252422715773777,-0.0746532949430514,0.0130000004));
#7013=CARTESIAN_POINT('',(-0.0252422715773777,-0.0746532949430514,0.0120000004));
#7014=CARTESIAN_POINT('',(0.,-0.0684221052,0.0130000004));
#7015=CARTESIAN_POINT('',(0.0252422715773777,-0.0746532949430514,0.0130000004));
#7016=CARTESIAN_POINT('',(0.0252422715773777,-0.0746532949430514,0.0130000004));
#7017=CARTESIAN_POINT('',(0.0252422715773777,-0.0746532949430514,0.0120000004));
#7018=CARTESIAN_POINT('',(0.,-0.0684221052,0.0120000004));
#7019=CARTESIAN_POINT('',(0.,0.,0.0130000004));
#7020=CARTESIAN_POINT('',(0.,-0.0746532949430514,0.0130000004));
#7021=CARTESIAN_POINT('',(0.,-0.0746532949430514,0.0130000004));
#7022=CARTESIAN_POINT('',(0.,-0.0684221052,-0.0130000004));
#7023=CARTESIAN_POINT('',(0.,-0.0684221052,-0.0120000004));
#7024=CARTESIAN_POINT('',(-0.0252422715773652,-0.0746532949430514,-0.0120000004000012));
#7025=CARTESIAN_POINT('',(0.0252422715773777,-0.0746532949430514,-0.0120000004));
#7026=CARTESIAN_POINT('',(0.0252422715773777,-0.0746532949430514,-0.0130000004));
#7027=CARTESIAN_POINT('',(0.0252422715773777,-0.0746532949430514,-0.0130000004));
#7028=CARTESIAN_POINT('',(0.,-0.0684221052,-0.0130000004));
#7029=CARTESIAN_POINT('',(-0.0252422715773777,-0.0746532949430514,-0.0130000004));
#7030=CARTESIAN_POINT('',(-0.0252422715773777,-0.0746532949430514,-0.0130000004));
#7031=CARTESIAN_POINT('',(0.,0.,-0.0130000004));
#7032=CARTESIAN_POINT('',(0.,-0.0746532949430514,-0.0130000004));
#7033=CARTESIAN_POINT('',(0.,-0.0746532949430514,-0.0130000004));
#7034=CARTESIAN_POINT('',(-0.03550000008,1.11917648088112E-18,-0.0100000004));
#7035=CARTESIAN_POINT('',(-0.03550000008,-0.0746532949430514,-0.0100000004));
#7036=CARTESIAN_POINT('',(-0.03550000008,-0.0578844846861027,-0.0100000004));
#7037=CARTESIAN_POINT('',(-0.03550000008,-0.0374221052,0.0100000004));
#7038=CARTESIAN_POINT('',(-0.03550000008,-0.0746532949430514,0.0100000004));
#7039=CARTESIAN_POINT('',(-0.03550000008,-0.0578844846861027,0.0100000004));
#7040=CARTESIAN_POINT('',(0.03550000008,-0.0374221052,-0.0100000004));
#7041=CARTESIAN_POINT('',(0.03550000008,-0.0746532949430514,-0.0100000004));
#7042=CARTESIAN_POINT('',(0.03550000008,-0.0578844846861027,-0.0100000004));
#7043=CARTESIAN_POINT('',(0.03550000008,-1.11917648088113E-18,0.0100000004));
#7044=CARTESIAN_POINT('',(0.03550000008,-0.0746532949430514,0.0100000004));
#7045=CARTESIAN_POINT('',(0.03550000008,-0.0578844846861027,0.0100000004));
#7046=CARTESIAN_POINT('',(0.,-0.0684221052,0.0120000004));
#7047=CARTESIAN_POINT('',(-0.0252422715773777,-0.0746532949430514,0.0120000004));
#7048=CARTESIAN_POINT('',(-0.0252422715773777,-0.0746532949430514,0.0117340892011008));
#7049=CARTESIAN_POINT('',(-0.0254741318712697,-0.0746532949430514,0.0112081301589468));
#7050=CARTESIAN_POINT('',(-0.0260068950976863,-0.0746532949430514,0.0110000004));
#7051=CARTESIAN_POINT('',(-0.0262711300553686,-0.0746532949430514,0.0110000004));
#7052=CARTESIAN_POINT('',(0.0262711300553686,-0.0746532949430514,0.0110000004));
#7053=CARTESIAN_POINT('',(0.0260068432764003,-0.0746532949430514,0.0110000004));
#7054=CARTESIAN_POINT('',(0.0254746601402995,-0.0746532949430514,0.0112068289794583));
#7055=CARTESIAN_POINT('',(0.0252422715773777,-0.0746532949430514,0.0117357303784197));
#7056=CARTESIAN_POINT('',(0.0252422715773777,-0.0746532949430514,0.0120000004));
#7057=CARTESIAN_POINT('',(0.,-0.0684221052,-0.0120000004));
#7058=CARTESIAN_POINT('',(-0.0262711300553686,-0.0746532949430514,-0.0110000004));
#7059=CARTESIAN_POINT('',(-0.0260041493105401,-0.0746532949430514,-0.0110000004));
#7060=CARTESIAN_POINT('',(-0.025474372265217,-0.0746532949430514,-0.0112087042075995));
#7061=CARTESIAN_POINT('',(-0.0252422715773772,-0.0746532949430514,-0.0117351103746127));
#7062=CARTESIAN_POINT('',(-0.0252422715773777,-0.0746532949430514,-0.0120000004000019));
#7063=CARTESIAN_POINT('',(0.0252422715773777,-0.0746532949430514,-0.0120000004));
#7064=CARTESIAN_POINT('',(0.0252422715773777,-0.0746532949430514,-0.0117324512139406));
#7065=CARTESIAN_POINT('',(0.0254742124828446,-0.0746532949430514,-0.0112095401021891));
#7066=CARTESIAN_POINT('',(0.0260054993852186,-0.0746532949430514,-0.0110000004));
#7067=CARTESIAN_POINT('',(0.0262711300553686,-0.0746532949430514,-0.0110000004));
#7068=CARTESIAN_POINT('',(0.03650000008,0.0532202,0.00799377303329589));
#7069=CARTESIAN_POINT('',(-0.00834780990288846,0.055739290033391,0.00799377303329589));
#7070=CARTESIAN_POINT('',(-0.0124910159490172,-0.0180229475260996,0.00799377303329588));
#7071=CARTESIAN_POINT('',(-0.00920784674600966,0.0404279004413879,0.00799377303329589));
#7072=CARTESIAN_POINT('',(0.,0.0403990320215515,0.00799377303329589));
#7073=CARTESIAN_POINT('',(-0.0070565442830717,0.0463143052920532,0.00799377303329589));
#7074=CARTESIAN_POINT('',(0.,0.06842,0.00799377303329589));
#7075=CARTESIAN_POINT('',(-0.0105921890504187,0.0477738844607493,0.00799377303329589));
#7076=CARTESIAN_POINT('',(-0.0770011542117716,0.0442631319913884,0.00799377303329589));
#7077=CARTESIAN_POINT('',(-0.0106041148871086,0.0405336272491669,0.00799377303329589));
#7078=CARTESIAN_POINT('',(-0.0144904743180211,-0.028655924125519,0.00799377303329588));
#7079=CARTESIAN_POINT('',(-0.0144904743180211,-0.028655924125519,0.00799377303329588));
#7080=CARTESIAN_POINT('',(-0.0479406149651572,-0.0267770382679513,0.00799377303329588));
#7081=CARTESIAN_POINT('',(-0.0150966619928097,-0.0333889120212214,0.00799377303329588));
#7082=CARTESIAN_POINT('',(0.,-0.0684221052,0.00799377303329588));
#7083=CARTESIAN_POINT('',(-0.00223898065795594,-0.0303403406237614,0.00799377303329588));
#7084=CARTESIAN_POINT('',(0.,-0.0180515951329767,0.00799377303329588));
#7085=CARTESIAN_POINT('',(0.03650000008,0.0532202,-0.0079937730332959));
#7086=CARTESIAN_POINT('',(0.00920631820296192,0.0404551133663912,-0.0079937730332959));
#7087=CARTESIAN_POINT('',(0.0124910159490172,-0.0180229475260996,-0.00799377303329591));
#7088=CARTESIAN_POINT('',(0.00920784674600966,0.0404279004413879,-0.0079937730332959));
#7089=CARTESIAN_POINT('',(0.,0.0403990320215515,-0.0079937730332959));
#7090=CARTESIAN_POINT('',(0.0070565442830717,0.0463143052920532,-0.0079937730332959));
#7091=CARTESIAN_POINT('',(0.,0.06842,-0.0079937730332959));
#7092=CARTESIAN_POINT('',(0.0105921890504172,0.0477738844607486,-0.0079937730332959));
#7093=CARTESIAN_POINT('',(0.0770011542117716,0.0442631319913884,-0.0079937730332959));
#7094=CARTESIAN_POINT('',(0.0106041148871086,0.0405336272491669,-0.0079937730332959));
#7095=CARTESIAN_POINT('',(0.0144904743180211,-0.028655924125519,-0.00799377303329591));
#7096=CARTESIAN_POINT('',(0.0144904743180211,-0.028655924125519,-0.00799377303329591));
#7097=CARTESIAN_POINT('',(0.0479406149651572,-0.0267770382679513,-0.00799377303329591));
#7098=CARTESIAN_POINT('',(0.0150966619928098,-0.0333889120212215,-0.00799377303329591));
#7099=CARTESIAN_POINT('',(0.,-0.0684221052,-0.00799377303329592));
#7100=CARTESIAN_POINT('',(0.00223898065795575,-0.0303403406237615,-0.00799377303329591));
#7101=CARTESIAN_POINT('',(0.,-0.0180515951329767,-0.00799377303329591));
#7102=CARTESIAN_POINT('',(0.03650000008,0.0836198,-0.01200000032));
#7103=CARTESIAN_POINT('',(0.0770011542117716,0.0442631319913884,-0.01200000032));
#7104=CARTESIAN_POINT('',(0.0135487072274815,0.0641694879715509,-0.01200000032));
#7105=CARTESIAN_POINT('',(0.0125890041486895,0.0608025080665035,-0.01200000032));
#7106=CARTESIAN_POINT('',(0.,0.06842,-0.01200000032));
#7107=CARTESIAN_POINT('',(7.67180601914802E-5,0.0537059481055745,-0.01200000032));
#7108=CARTESIAN_POINT('',(-7.79740982756669E-5,0.0537059481055745,-0.01200000032));
#7109=CARTESIAN_POINT('',(-7.67180601914596E-5,0.0537059481055745,-0.01200000032));
#7110=CARTESIAN_POINT('',(0.,0.06842,-0.01200000032));
#7111=CARTESIAN_POINT('',(-0.0125890041486895,0.0608025080665034,-0.01200000032));
#7112=CARTESIAN_POINT('',(-0.0770011542117716,0.0442631319913884,-0.01200000032));
#7113=CARTESIAN_POINT('',(-0.0135487072274815,0.0641694879715509,-0.01200000032));
#7114=CARTESIAN_POINT('',(0.,0.06842,-0.01200000032));
#7115=CARTESIAN_POINT('',(0.,0.06842,-0.01200000032));
#7116=CARTESIAN_POINT('',(-0.0132,0.06842,-0.01200000032));
#7117=CARTESIAN_POINT('',(-0.0770011542117716,0.0442631319913884,-0.01200000032));
#7118=CARTESIAN_POINT('',(-0.0145028549779767,0.0638701519225609,-0.01200000032));
#7119=CARTESIAN_POINT('',(-0.0145028549779767,0.0638701519225609,-0.01100000032));
#7120=CARTESIAN_POINT('',(-0.0145028549779767,0.0638701519225609,0.01100000032));
#7121=CARTESIAN_POINT('',(-0.0770011542117716,0.0442631319913884,-0.01100000032));
#7122=CARTESIAN_POINT('',(-0.0135575831556183,0.0605538020003595,-0.01100000032));
#7123=CARTESIAN_POINT('',(-0.0135575831556183,0.0605538020003595,-0.0110000003199999));
#7124=CARTESIAN_POINT('',(-0.0132893606164165,0.059509216620179,-0.010616320417549));
#7125=CARTESIAN_POINT('',(-0.0128216806843899,0.0574792137206106,-0.00966529500091684));
#7126=CARTESIAN_POINT('',(-0.0122598045310854,0.0543864981658248,-0.00828932161082693));
#7127=CARTESIAN_POINT('',(-0.0118307350725021,0.0511196604769446,-0.00726764709369388));
#7128=CARTESIAN_POINT('',(-0.0116516459867705,0.0488721502335481,-0.0069937730332959));
#7129=CARTESIAN_POINT('',(-0.0115907945846862,0.0477210925397055,-0.0069937730332959));
#7130=CARTESIAN_POINT('',(-0.0115907945846862,0.0477210925397055,-0.0069937730332959));
#7131=CARTESIAN_POINT('',(-0.0770011542117716,0.0442631319913884,-0.0069937730332959));
#7132=CARTESIAN_POINT('',(-0.0116025410900705,0.0405897085940067,-0.0069937730332959));
#7133=CARTESIAN_POINT('',(-0.0116025410900705,0.0405897085940067,-0.01200000032));
#7134=CARTESIAN_POINT('',(-0.0116025410900705,0.0405897085940067,0.00699377303329589));
#7135=CARTESIAN_POINT('',(-0.0770011542117716,0.0442631319913884,0.00699377303329589));
#7136=CARTESIAN_POINT('',(-0.0115907945846863,0.0477210925397086,0.00699377303329589));
#7137=CARTESIAN_POINT('',(-0.0115907945846864,0.0477210925397086,0.00699377303329589));
#7138=CARTESIAN_POINT('',(-0.0116516459867707,0.048872150233551,0.00699377303329614));
#7139=CARTESIAN_POINT('',(-0.0118307350725023,0.0511196604769469,0.00726764709369443));
#7140=CARTESIAN_POINT('',(-0.0122598045310857,0.0543864981658262,0.00828932161082755));
#7141=CARTESIAN_POINT('',(-0.01282168068439,0.0574792137206114,0.00966529500091711));
#7142=CARTESIAN_POINT('',(-0.0132893606164165,0.0595092166201793,0.0106163204175492));
#7143=CARTESIAN_POINT('',(-0.0135575831556184,0.0605538020003596,0.01100000032));
#7144=CARTESIAN_POINT('',(-0.0135575831556183,0.0605538020003596,0.01100000032));
#7145=CARTESIAN_POINT('',(-0.0770011542117716,0.0442631319913884,0.01100000032));
#7146=CARTESIAN_POINT('',(0.0770011542117716,0.0442631319913884,-0.01200000032));
#7147=CARTESIAN_POINT('',(0.0115907945846862,0.0477210925397055,-0.0069937730332959));
#7148=CARTESIAN_POINT('',(0.0116516459867705,0.0488721502335482,-0.0069937730332959));
#7149=CARTESIAN_POINT('',(0.0118307350725021,0.0511196604769446,-0.00726764709369388));
#7150=CARTESIAN_POINT('',(0.0122598045310854,0.0543864981658248,-0.00828932161082697));
#7151=CARTESIAN_POINT('',(0.0128216806843899,0.0574792137206107,-0.00966529500091678));
#7152=CARTESIAN_POINT('',(0.0132893606164165,0.0595092166201791,-0.0106163204175491));
#7153=CARTESIAN_POINT('',(0.0135575831556184,0.0605538020003596,-0.01100000032));
#7154=CARTESIAN_POINT('',(0.0115907945846862,0.0477210925397055,-0.0069937730332959));
#7155=CARTESIAN_POINT('',(0.0135575831556183,0.0605538020003596,-0.01100000032));
#7156=CARTESIAN_POINT('',(0.0770011542117716,0.0442631319913884,-0.01100000032));
#7157=CARTESIAN_POINT('',(0.0145028549779767,0.0638701519225609,-0.01100000032));
#7158=CARTESIAN_POINT('',(0.0145028549779767,0.0638701519225609,-0.01200000032));
#7159=CARTESIAN_POINT('',(0.0145028549779767,0.0638701519225609,0.01100000032));
#7160=CARTESIAN_POINT('',(0.0770011542117716,0.0442631319913884,0.01100000032));
#7161=CARTESIAN_POINT('',(0.0135575831556183,0.0605538020003596,0.01100000032));
#7162=CARTESIAN_POINT('',(0.0135575831556184,0.0605538020003596,0.01100000032));
#7163=CARTESIAN_POINT('',(0.0132893606164165,0.0595092166201791,0.0106163204175491));
#7164=CARTESIAN_POINT('',(0.0128216806843899,0.0574792137206106,0.00966529500091686));
#7165=CARTESIAN_POINT('',(0.0122598045310854,0.0543864981658248,0.00828932161082694));
#7166=CARTESIAN_POINT('',(0.0118307350725021,0.0511196604769446,0.00726764709369388));
#7167=CARTESIAN_POINT('',(0.0116516459867705,0.0488721502335482,0.00699377303329589));
#7168=CARTESIAN_POINT('',(0.0115907945846862,0.0477210925397055,0.00699377303329589));
#7169=CARTESIAN_POINT('',(0.0115907945846862,0.0477210925397055,0.00699377303329589));
#7170=CARTESIAN_POINT('',(0.0770011542117716,0.0442631319913884,0.00699377303329589));
#7171=CARTESIAN_POINT('',(0.0116025410900705,0.0405897085940067,0.00699377303329589));
#7172=CARTESIAN_POINT('',(0.0116025410900705,0.0405897085940067,-0.01200000032));
#7173=CARTESIAN_POINT('',(0.0116025410900705,0.0405897085940067,-0.0069937730332959));
#7174=CARTESIAN_POINT('',(0.0770011542117716,0.0442631319913884,-0.0069937730332959));
#7175=CARTESIAN_POINT('',(0.03650000008,0.0836198,0.01200000032));
#7176=CARTESIAN_POINT('',(-0.0770011542117716,0.0442631319913884,0.01200000032));
#7177=CARTESIAN_POINT('',(-0.0135487072274815,0.0641694879715509,0.01200000032));
#7178=CARTESIAN_POINT('',(-0.0125890041486895,0.0608025080665035,0.01200000032));
#7179=CARTESIAN_POINT('',(0.,0.06842,0.01200000032));
#7180=CARTESIAN_POINT('',(-7.67180601910061E-5,0.0537059481055745,0.01200000032));
#7181=CARTESIAN_POINT('',(0.03650000008,0.0537059481055745,0.01200000032));
#7182=CARTESIAN_POINT('',(7.67180601909946E-5,0.0537059481055745,0.01200000032));
#7183=CARTESIAN_POINT('',(0.,0.06842,0.01200000032));
#7184=CARTESIAN_POINT('',(0.0125890041486895,0.0608025080665034,0.01200000032));
#7185=CARTESIAN_POINT('',(0.0770011542117716,0.0442631319913884,0.01200000032));
#7186=CARTESIAN_POINT('',(0.0135487072274815,0.0641694879715509,0.01200000032));
#7187=CARTESIAN_POINT('',(0.,0.06842,0.01200000032));
#7188=CARTESIAN_POINT('',(0.,0.06842,0.01200000032));
#7189=CARTESIAN_POINT('',(-0.0132,0.06842,0.01200000032));
#7190=CARTESIAN_POINT('',(0.03650000008,0.0532202,0.00799377303329589));
#7191=CARTESIAN_POINT('',(0.0124894750029619,-0.017995513788137,0.00799377303329588));
#7192=CARTESIAN_POINT('',(0.00920784674600963,0.040427900441388,0.00799377303329589));
#7193=CARTESIAN_POINT('',(0.0124910159490172,-0.0180229475260995,0.00799377303329588));
#7194=CARTESIAN_POINT('',(0.,-0.0180515951329767,0.00799377303329588));
#7195=CARTESIAN_POINT('',(0.00223898065795594,-0.0303403406237614,0.00799377303329588));
#7196=CARTESIAN_POINT('',(0.,-0.0684221052,0.00799377303329588));
#7197=CARTESIAN_POINT('',(0.0150966619928115,-0.0333889120212222,0.00799377303329588));
#7198=CARTESIAN_POINT('',(0.0479406149651572,-0.0267770382679513,0.00799377303329588));
#7199=CARTESIAN_POINT('',(0.0144904743180211,-0.028655924125519,0.00799377303329588));
#7200=CARTESIAN_POINT('',(0.00997520014598791,0.0517303087616774,0.00799377303329589));
#7201=CARTESIAN_POINT('',(0.0106041148871086,0.0405336272491669,0.00799377303329589));
#7202=CARTESIAN_POINT('',(0.0770011542117716,0.0442631319913884,0.00799377303329589));
#7203=CARTESIAN_POINT('',(0.0105921890504172,0.0477738844607486,0.00799377303329589));
#7204=CARTESIAN_POINT('',(0.,0.06842,0.00799377303329589));
#7205=CARTESIAN_POINT('',(0.0070565442830717,0.0463143052920532,0.00799377303329589));
#7206=CARTESIAN_POINT('',(0.,0.0403990320215515,0.00799377303329589));
#7207=CARTESIAN_POINT('',(0.03650000008,0.0532202,-0.0079937730332959));
#7208=CARTESIAN_POINT('',(-0.00834780990288846,0.055739290033391,-0.0079937730332959));
#7209=CARTESIAN_POINT('',(-0.00920784674600963,0.0404279004413879,-0.0079937730332959));
#7210=CARTESIAN_POINT('',(-0.0124910159490172,-0.0180229475260996,-0.00799377303329591));
#7211=CARTESIAN_POINT('',(0.,-0.0180515951329767,-0.00799377303329591));
#7212=CARTESIAN_POINT('',(-0.00223898065795575,-0.0303403406237615,-0.00799377303329591));
#7213=CARTESIAN_POINT('',(0.,-0.0684221052,-0.00799377303329592));
#7214=CARTESIAN_POINT('',(-0.0150966619928098,-0.0333889120212215,-0.00799377303329591));
#7215=CARTESIAN_POINT('',(-0.0479406149651572,-0.0267770382679513,-0.00799377303329591));
#7216=CARTESIAN_POINT('',(-0.0144904743180211,-0.028655924125519,-0.00799377303329591));
#7217=CARTESIAN_POINT('',(-0.00974560658703515,0.0558178039161666,-0.0079937730332959));
#7218=CARTESIAN_POINT('',(-0.0106041148871086,0.0405336272491669,-0.0079937730332959));
#7219=CARTESIAN_POINT('',(-0.0770011542117716,0.0442631319913884,-0.0079937730332959));
#7220=CARTESIAN_POINT('',(-0.0105921890504172,0.0477738844607486,-0.0079937730332959));
#7221=CARTESIAN_POINT('',(0.,0.06842,-0.0079937730332959));
#7222=CARTESIAN_POINT('',(-0.0070565442830717,0.0463143052920532,-0.0079937730332959));
#7223=CARTESIAN_POINT('',(0.,0.0403990320215515,-0.0079937730332959));
#7224=CARTESIAN_POINT('',(-0.0479406149651572,-0.0267770382679513,-0.01200000032));
#7225=CARTESIAN_POINT('',(-0.0479406149651572,-0.0267770382679513,-0.0100000004));
#7226=CARTESIAN_POINT('',(-0.0208497874735458,-0.0447359762231199,-0.0100000004));
#7227=CARTESIAN_POINT('',(-0.0358713299351814,-0.0569559836690592,-0.0100000004));
#7228=CARTESIAN_POINT('',(-0.0358713299351814,-0.0569559836690592,-0.01200000032));
#7229=CARTESIAN_POINT('',(-0.0358713299351814,-0.0569559836690592,0.0100000004));
#7230=CARTESIAN_POINT('',(-0.0479406149651572,-0.0267770382679513,0.0100000004));
#7231=CARTESIAN_POINT('',(-0.0208497874735458,-0.0447359762231199,0.0100000004));
#7232=CARTESIAN_POINT('',(-0.0208497874735458,-0.0447359762231199,0.0100000004));
#7233=CARTESIAN_POINT('',(-0.0196876809355329,-0.0429829534203924,0.00944920348110594));
#7234=CARTESIAN_POINT('',(-0.0177795515520167,-0.039402141360841,0.00790667524421345));
#7235=CARTESIAN_POINT('',(-0.0165079106461819,-0.0353321005215666,0.00699377303329588));
#7236=CARTESIAN_POINT('',(-0.0160769945899836,-0.0331915595474134,0.00699377303329588));
#7237=CARTESIAN_POINT('',(-0.0160769945899836,-0.0331915595474134,0.00699377303329588));
#7238=CARTESIAN_POINT('',(-0.0479406149651572,-0.0267770382679513,0.00699377303329588));
#7239=CARTESIAN_POINT('',(-0.015488900520983,-0.0285998427806792,0.00699377303329588));
#7240=CARTESIAN_POINT('',(-0.015488900520983,-0.0285998427806792,-0.01200000032));
#7241=CARTESIAN_POINT('',(-0.015488900520983,-0.0285998427806792,-0.00699377303329591));
#7242=CARTESIAN_POINT('',(-0.0479406149651572,-0.0267770382679513,-0.00699377303329591));
#7243=CARTESIAN_POINT('',(-0.0160769945899837,-0.0331915595474134,-0.00699377303329591));
#7244=CARTESIAN_POINT('',(-0.0160769945899837,-0.0331915595474134,-0.00699377303329591));
#7245=CARTESIAN_POINT('',(-0.0165079106461819,-0.0353321005215667,-0.00699377303329591));
#7246=CARTESIAN_POINT('',(-0.0177795515520167,-0.0394021413608411,-0.00790667524421339));
#7247=CARTESIAN_POINT('',(-0.0196876809355329,-0.0429829534203924,-0.00944920348110595));
#7248=CARTESIAN_POINT('',(-0.0208497874735458,-0.0447359762231199,-0.0100000004));
#7249=CARTESIAN_POINT('',(0.,0.06842,-0.01200000032));
#7250=CARTESIAN_POINT('',(0.,0.06842,-0.01100000032));
#7251=CARTESIAN_POINT('',(0.,0.06842,0.01100000032));
#7252=CARTESIAN_POINT('',(0.0479406149651572,-0.0267770382679513,-0.01200000032));
#7253=CARTESIAN_POINT('',(0.0479406149651572,-0.0267770382679513,0.0100000004));
#7254=CARTESIAN_POINT('',(0.0208497874735458,-0.0447359762231199,0.0100000004));
#7255=CARTESIAN_POINT('',(0.0358713299351814,-0.0569559836690592,0.0100000004));
#7256=CARTESIAN_POINT('',(0.0358713299351814,-0.0569559836690592,-0.01200000032));
#7257=CARTESIAN_POINT('',(0.0358713299351814,-0.0569559836690592,-0.0100000004));
#7258=CARTESIAN_POINT('',(0.0479406149651572,-0.0267770382679513,-0.0100000004));
#7259=CARTESIAN_POINT('',(0.0208497874735458,-0.0447359762231199,-0.0100000004));
#7260=CARTESIAN_POINT('',(0.0208497874735458,-0.0447359762231199,-0.0100000004));
#7261=CARTESIAN_POINT('',(0.0196876809355329,-0.0429829534203924,-0.00944920348110595));
#7262=CARTESIAN_POINT('',(0.0177795515520167,-0.0394021413608411,-0.0079066752442134));
#7263=CARTESIAN_POINT('',(0.0165079106461819,-0.0353321005215667,-0.00699377303329591));
#7264=CARTESIAN_POINT('',(0.0160769945899837,-0.0331915595474134,-0.00699377303329591));
#7265=CARTESIAN_POINT('',(0.0160769945899837,-0.0331915595474134,-0.00699377303329591));
#7266=CARTESIAN_POINT('',(0.0479406149651572,-0.0267770382679513,-0.00699377303329591));
#7267=CARTESIAN_POINT('',(0.015488900520983,-0.0285998427806792,-0.00699377303329591));
#7268=CARTESIAN_POINT('',(0.015488900520983,-0.0285998427806792,-0.01200000032));
#7269=CARTESIAN_POINT('',(0.015488900520983,-0.0285998427806792,0.00699377303329588));
#7270=CARTESIAN_POINT('',(0.0479406149651572,-0.0267770382679513,0.00699377303329588));
#7271=CARTESIAN_POINT('',(0.0160769945899843,-0.0331915595474165,0.00699377303329588));
#7272=CARTESIAN_POINT('',(0.0160769945899843,-0.0331915595474165,0.00699377303329588));
#7273=CARTESIAN_POINT('',(0.0165079106461826,-0.0353321005215691,0.00699377303329633));
#7274=CARTESIAN_POINT('',(0.0177795515520174,-0.0394021413608423,0.00790667524421404));
#7275=CARTESIAN_POINT('',(0.0196876809355332,-0.0429829534203928,0.00944920348110608));
#7276=CARTESIAN_POINT('',(0.0208497874735458,-0.0447359762231199,0.0100000004));
#7277=CARTESIAN_POINT('',(0.0138387927084345,0.000777321452246679,-0.01200000032));
#7278=CARTESIAN_POINT('',(0.0116025410900705,0.0405897085940067,-0.0069937730332959));
#7279=CARTESIAN_POINT('',(0.0138387927084345,0.000777321452246678,0.00699377303329589));
#7280=CARTESIAN_POINT('',(-0.0138387927084345,0.000777321452246679,-0.01200000032));
#7281=CARTESIAN_POINT('',(-0.0138387927084345,0.000777321452246679,-0.00699377303329591));
#7282=CARTESIAN_POINT('',(-0.0116025410900705,0.0405897085940067,0.00699377303329589));
#7283=CARTESIAN_POINT('',(0.,0.06842,-0.01200000032));
#7284=CARTESIAN_POINT('',(0.,0.06842,-0.0120000004));
#7285=CARTESIAN_POINT('',(-0.011,0.06842,-0.0120000004));
#7286=CARTESIAN_POINT('',(0.,0.06842,0.0120000004));
#7287=CARTESIAN_POINT('',(0.011,0.06842,0.0120000004));
#7288=CARTESIAN_POINT('',(-0.010444143618364,0.000586644879791539,0.0016));
#7289=CARTESIAN_POINT('',(-0.008207892,0.0403990320215515,0.0016));
#7290=CARTESIAN_POINT('',(-0.008207892,0.0403990320215515,0.0026));
#7291=CARTESIAN_POINT('',(-0.008207892,0.0403990320215515,0.00699377303329589));
#7292=CARTESIAN_POINT('',(-0.010444143618364,0.000586644879791538,0.00699377303329588));
#7293=CARTESIAN_POINT('',(-0.0114910488,-0.0180515951329767,0.00699377303329588));
#7294=CARTESIAN_POINT('',(-0.0114910488,-0.0180515951329767,0.0016));
#7295=CARTESIAN_POINT('',(-0.0114910488,-0.0180515951329767,0.0026));
#7296=CARTESIAN_POINT('',(-0.010444143618364,0.000586644879791539,0.0026));
#7297=CARTESIAN_POINT('',(0.,0.0403990320215515,0.0016));
#7298=CARTESIAN_POINT('',(-7.73280731427145E-5,0.0486065597524074,0.00790817554892985));
#7299=CARTESIAN_POINT('',(-0.00248654459668742,0.0485838610692401,0.00789166359185419));
#7300=CARTESIAN_POINT('',(-0.0047401145182197,0.0475210284454703,0.00699377303329588));
#7301=CARTESIAN_POINT('',(-0.00629018600225436,0.0456718918851082,0.00699377303329589));
#7302=CARTESIAN_POINT('',(-7.73280731427158E-5,0.0486065597524074,0.00790817554893012));
#7303=CARTESIAN_POINT('',(-0.00629018600225436,0.0456718918851082,0.00699377303329589));
#7304=CARTESIAN_POINT('',(0.,0.0403990320215515,0.00699377303329589));
#7305=CARTESIAN_POINT('',(0.,0.0403990320215515,0.0026));
#7306=CARTESIAN_POINT('',(0.008207892,0.0403990320215515,0.0026));
#7307=CARTESIAN_POINT('',(0.008207892,0.0403990320215515,0.0016));
#7308=CARTESIAN_POINT('',(0.008207892,0.0403990320215515,0.00699377303329589));
#7309=CARTESIAN_POINT('',(0.,0.0403990320215515,0.00699377303329589));
#7310=CARTESIAN_POINT('',(0.00629018600225437,0.0456718918851082,0.00699377303329589));
#7311=CARTESIAN_POINT('',(0.00629018600225437,0.0456718918851082,0.00699377303329589));
#7312=CARTESIAN_POINT('',(0.00474011451821985,0.0475210284454701,0.00699377303329588));
#7313=CARTESIAN_POINT('',(0.00248654459668787,0.0485838610692399,0.00789166359185404));
#7314=CARTESIAN_POINT('',(7.73280731434021E-5,0.0486065597524074,0.00790817554892985));
#7315=CARTESIAN_POINT('',(7.73280731434013E-5,0.0486065597524074,0.00790817554892985));
#7316=CARTESIAN_POINT('',(7.73280731434192E-5,0.0486065597524074,0.00790817554893013));
#7317=CARTESIAN_POINT('',(2.57775496670895E-5,0.048607045441007,0.00790817554893013));
#7318=CARTESIAN_POINT('',(-2.57775496664051E-5,0.048607045441007,0.00790817554893013));
#7319=CARTESIAN_POINT('',(-7.73280731427348E-5,0.0486065597524074,0.00790817554893013));
#7320=CARTESIAN_POINT('',(0.010444143618364,0.000586644879791539,0.0016));
#7321=CARTESIAN_POINT('',(0.0114910488,-0.0180515951329767,0.0016));
#7322=CARTESIAN_POINT('',(0.0114910488,-0.0180515951329767,0.0026));
#7323=CARTESIAN_POINT('',(0.0114910488,-0.0180515951329767,0.00699377303329588));
#7324=CARTESIAN_POINT('',(0.008207892,0.0403990320215515,0.00699377303329589));
#7325=CARTESIAN_POINT('',(0.0114910488,-0.0180515951329768,0.0026));
#7326=CARTESIAN_POINT('',(0.,-0.0180515951329767,0.0016));
#7327=CARTESIAN_POINT('',(0.,-0.0180515951329767,0.00699377303329588));
#7328=CARTESIAN_POINT('',(-0.00205973384739541,-0.029356536486291,0.00699377303329588));
#7329=CARTESIAN_POINT('',(-0.00205973384739541,-0.029356536486291,0.00699377303329588));
#7330=CARTESIAN_POINT('',(-0.000686577949131805,-0.029606722276116,0.00699377303329588));
#7331=CARTESIAN_POINT('',(0.00068657794913181,-0.029606722276116,0.00699377303329588));
#7332=CARTESIAN_POINT('',(0.00205973384739542,-0.029356536486291,0.00699377303329588));
#7333=CARTESIAN_POINT('',(0.00205973384739541,-0.029356536486291,0.00699377303329588));
#7334=CARTESIAN_POINT('',(0.,-0.0180515951329767,0.00699377303329588));
#7335=CARTESIAN_POINT('',(0.,-0.0180515951329767,0.0026));
#7336=CARTESIAN_POINT('',(0.,0.,0.0016));
#7337=CARTESIAN_POINT('',(0.00720946579703808,0.0403429506767117,0.0016));
#7338=CARTESIAN_POINT('',(0.0104910129546957,-0.018079019727579,0.0016));
#7339=CARTESIAN_POINT('',(0.00720784085825531,0.0403718797522103,0.0016));
#7340=CARTESIAN_POINT('',(0.,0.0403990320215515,0.0016));
#7341=CARTESIAN_POINT('',(-0.00720784085825531,0.0403718797522103,0.0016));
#7342=CARTESIAN_POINT('',(-0.00944571741540203,0.000530563534951791,0.0016));
#7343=CARTESIAN_POINT('',(-0.0104910129546957,-0.018079019727579,0.0016));
#7344=CARTESIAN_POINT('',(0.,-0.0180515951329767,0.0016));
#7345=CARTESIAN_POINT('',(-0.010444143618364,0.000586644879791539,-0.0016));
#7346=CARTESIAN_POINT('',(-0.0114910488,-0.0180515951329767,-0.0016));
#7347=CARTESIAN_POINT('',(-0.0114910488,-0.0180515951329767,-0.0026));
#7348=CARTESIAN_POINT('',(-0.0114910488,-0.0180515951329767,-0.00699377303329591));
#7349=CARTESIAN_POINT('',(-0.010444143618364,0.000586644879791539,-0.00699377303329591));
#7350=CARTESIAN_POINT('',(-0.008207892,0.0403990320215515,-0.0069937730332959));
#7351=CARTESIAN_POINT('',(-0.008207892,0.0403990320215515,-0.0016));
#7352=CARTESIAN_POINT('',(-0.008207892,0.0403990320215515,-0.0026));
#7353=CARTESIAN_POINT('',(-0.0114910488,-0.0180515951329768,-0.0026));
#7354=CARTESIAN_POINT('',(0.,-0.0180515951329767,-0.0016));
#7355=CARTESIAN_POINT('',(0.0114910488,-0.0180515951329767,-0.0016));
#7356=CARTESIAN_POINT('',(0.0114910488,-0.0180515951329767,-0.0026));
#7357=CARTESIAN_POINT('',(0.0114910488,-0.0180515951329767,-0.00699377303329591));
#7358=CARTESIAN_POINT('',(0.,-0.0180515951329767,-0.00699377303329591));
#7359=CARTESIAN_POINT('',(0.00205973384739524,-0.029356536486291,-0.00699377303329591));
#7360=CARTESIAN_POINT('',(0.00205973384739524,-0.029356536486291,-0.00699377303329591));
#7361=CARTESIAN_POINT('',(0.000686577949131747,-0.029606722276116,-0.00699377303329591));
#7362=CARTESIAN_POINT('',(-0.000686577949131747,-0.029606722276116,-0.00699377303329591));
#7363=CARTESIAN_POINT('',(-0.00205973384739524,-0.029356536486291,-0.00699377303329591));
#7364=CARTESIAN_POINT('',(-0.00205973384739524,-0.029356536486291,-0.00699377303329591));
#7365=CARTESIAN_POINT('',(0.,-0.0180515951329767,-0.00699377303329591));
#7366=CARTESIAN_POINT('',(0.,-0.0180515951329767,-0.0026));
#7367=CARTESIAN_POINT('',(0.010444143618364,0.000586644879791539,-0.0016));
#7368=CARTESIAN_POINT('',(0.008207892,0.0403990320215515,-0.0016));
#7369=CARTESIAN_POINT('',(0.008207892,0.0403990320215515,-0.0026));
#7370=CARTESIAN_POINT('',(0.008207892,0.0403990320215515,-0.0069937730332959));
#7371=CARTESIAN_POINT('',(0.0114910488,-0.0180515951329767,-0.00699377303329591));
#7372=CARTESIAN_POINT('',(0.010444143618364,0.000586644879791539,-0.0026));
#7373=CARTESIAN_POINT('',(0.,0.0403990320215515,-0.0016));
#7374=CARTESIAN_POINT('',(7.73280731449155E-5,0.0486065597524074,-0.00790817554892985));
#7375=CARTESIAN_POINT('',(0.00248654459668886,0.0485838610692395,-0.00789166359185372));
#7376=CARTESIAN_POINT('',(0.00474011451822018,0.0475210284454697,-0.00699377303329589));
#7377=CARTESIAN_POINT('',(0.00629018600225436,0.0456718918851082,-0.0069937730332959));
#7378=CARTESIAN_POINT('',(7.73280731449167E-5,0.0486065597524074,-0.00790817554893012));
#7379=CARTESIAN_POINT('',(0.00629018600225436,0.0456718918851082,-0.0069937730332959));
#7380=CARTESIAN_POINT('',(0.,0.0403990320215515,-0.0069937730332959));
#7381=CARTESIAN_POINT('',(0.,0.0403990320215515,-0.0026));
#7382=CARTESIAN_POINT('',(0.,0.0403990320215515,-0.0069937730332959));
#7383=CARTESIAN_POINT('',(-0.00629018600225436,0.0456718918851082,-0.0069937730332959));
#7384=CARTESIAN_POINT('',(-0.00629018600225436,0.0456718918851082,-0.0069937730332959));
#7385=CARTESIAN_POINT('',(-0.00474011451822014,0.0475210284454698,-0.00699377303329589));
#7386=CARTESIAN_POINT('',(-0.00248654459668875,0.0485838610692395,-0.00789166359185376));
#7387=CARTESIAN_POINT('',(-7.73280731447373E-5,0.0486065597524074,-0.00790817554892985));
#7388=CARTESIAN_POINT('',(-7.73280731447357E-5,0.0486065597524074,-0.00790817554892985));
#7389=CARTESIAN_POINT('',(-7.73280731447314E-5,0.0486065597524073,-0.00790817554893013));
#7390=CARTESIAN_POINT('',(-2.57775496672397E-5,0.048607045441007,-0.00790817554893013));
#7391=CARTESIAN_POINT('',(2.57775496674173E-5,0.048607045441007,-0.00790817554893013));
#7392=CARTESIAN_POINT('',(7.7328073144909E-5,0.0486065597524073,-0.00790817554893013));
#7393=CARTESIAN_POINT('',(0.,0.,-0.0016));
#7394=CARTESIAN_POINT('',(0.00944571741540203,0.000530563534951791,-0.0016));
#7395=CARTESIAN_POINT('',(0.00720784085825524,0.0403718797522103,-0.0016));
#7396=CARTESIAN_POINT('',(0.0104910129546957,-0.018079019727579,-0.0016));
#7397=CARTESIAN_POINT('',(0.,-0.0180515951329767,-0.0016));
#7398=CARTESIAN_POINT('',(-0.0104910129546957,-0.018079019727579,-0.0016));
#7399=CARTESIAN_POINT('',(-0.00720946579703808,0.0403429506767117,-0.0016));
#7400=CARTESIAN_POINT('',(-0.00720784085825531,0.0403718797522103,-0.0016));
#7401=CARTESIAN_POINT('',(0.,0.0403990320215515,-0.0016));
#7402=CARTESIAN_POINT('',(0.,0.06842,-0.0179937730332959));
#7403=CARTESIAN_POINT('',(7.87045304632302E-5,0.0529340922159572,-0.0116357978393905));
#7404=CARTESIAN_POINT('',(8.12506199999854E-5,0.0519321483087437,-0.0104194415588719));
#7405=CARTESIAN_POINT('',(8.43928020623833E-5,0.0506415015783407,-0.00944944180385271));
#7406=CARTESIAN_POINT('',(8.76647539293995E-5,0.0492073273028014,-0.00882504461561704));
#7407=CARTESIAN_POINT('',(7.87045304645403E-5,0.0529340922159572,-0.0116357978393905));
#7408=CARTESIAN_POINT('',(8.76647539280907E-5,0.0492073273028014,-0.00882504461561705));
#7409=CARTESIAN_POINT('',(0.,0.06842,-0.0116357978393905));
#7410=CARTESIAN_POINT('',(0.0132493773070601,0.060402922273412,-0.0116357978393905));
#7411=CARTESIAN_POINT('',(0.0132493773070601,0.060402922273412,-0.0116357978393905));
#7412=CARTESIAN_POINT('',(0.0129415944843386,0.0593692724324227,-0.0113058495927241));
#7413=CARTESIAN_POINT('',(0.0123626737236228,0.0573528398286717,-0.0104792531774306));
#7414=CARTESIAN_POINT('',(0.0113509423413671,0.0532843354740351,-0.00880854902741558));
#7415=CARTESIAN_POINT('',(0.0108078930523586,0.0500332694111275,-0.0079937730332959));
#7416=CARTESIAN_POINT('',(0.0105921890504172,0.0477738844607486,-0.0079937730332959));
#7417=CARTESIAN_POINT('',(0.0070565442830717,0.0463143052920532,-0.0079937730332959));
#7418=CARTESIAN_POINT('',(0.00617530299378753,0.0472946724703006,-0.00799377303329589));
#7419=CARTESIAN_POINT('',(0.00398690985736663,0.0487289177719894,-0.00843903646475693));
#7420=CARTESIAN_POINT('',(0.00140037055543791,0.0491971093619505,-0.00881798832068754));
#7421=CARTESIAN_POINT('',(8.76647097163739E-5,0.0492073466820214,-0.00882505305278234));
#7422=CARTESIAN_POINT('',(0.03650000008,0.0452155333197847,-0.0179937730332959));
#7423=CARTESIAN_POINT('',(-7.87045304632302E-5,0.0529340922159572,-0.0116357978393905));
#7424=CARTESIAN_POINT('',(-8.12506199999854E-5,0.0519321483087437,-0.0104194415588719));
#7425=CARTESIAN_POINT('',(-8.43928020623833E-5,0.0506415015783407,-0.00944944180385271));
#7426=CARTESIAN_POINT('',(-8.76647539293995E-5,0.0492073273028014,-0.00882504461561704));
#7427=CARTESIAN_POINT('',(-7.87045304645403E-5,0.0529340922159572,-0.0116357978393905));
#7428=CARTESIAN_POINT('',(-8.76647539283538E-5,0.0492073273028014,-0.00882504461561705));
#7429=CARTESIAN_POINT('',(0.03650000008,0.0529340922159572,-0.0116357978393905));
#7430=CARTESIAN_POINT('',(8.76647539280948E-5,0.0492073273028014,-0.00882504461561705));
#7431=CARTESIAN_POINT('',(2.92215846425317E-5,0.0492078331572327,-0.00882526484971964));
#7432=CARTESIAN_POINT('',(-2.92215846429342E-5,0.0492078331572327,-0.00882526484971964));
#7433=CARTESIAN_POINT('',(-8.76647539283029E-5,0.0492073273028014,-0.00882504461561705));
#7434=CARTESIAN_POINT('',(0.,0.06842,-0.0179937730332959));
#7435=CARTESIAN_POINT('',(-0.0105921890504172,0.0477738844607486,-0.0079937730332959));
#7436=CARTESIAN_POINT('',(-0.0108078930523586,0.0500332694111275,-0.0079937730332959));
#7437=CARTESIAN_POINT('',(-0.0113509423413671,0.0532843354740351,-0.0088085490274156));
#7438=CARTESIAN_POINT('',(-0.0123626737236227,0.0573528398286717,-0.0104792531774306));
#7439=CARTESIAN_POINT('',(-0.0129415944843386,0.0593692724324227,-0.0113058495927241));
#7440=CARTESIAN_POINT('',(-0.0132493773070601,0.0604029222734119,-0.0116357978393905));
#7441=CARTESIAN_POINT('',(-0.0132493773070601,0.0604029222734119,-0.0116357978393905));
#7442=CARTESIAN_POINT('',(0.,0.06842,-0.0116357978393905));
#7443=CARTESIAN_POINT('',(-8.76647097176486E-5,0.0492073466820214,-0.00882505305278234));
#7444=CARTESIAN_POINT('',(-0.00140037055543896,0.0491971093619503,-0.00881798832068744));
#7445=CARTESIAN_POINT('',(-0.00398690985736713,0.0487289177719891,-0.0084390364647568));
#7446=CARTESIAN_POINT('',(-0.00617530299378768,0.0472946724703004,-0.00799377303329589));
#7447=CARTESIAN_POINT('',(-0.0070565442830717,0.0463143052920532,-0.0079937730332959));
#7448=CARTESIAN_POINT('',(0.,0.06842,0.0179937730332959));
#7449=CARTESIAN_POINT('',(-7.87045304628983E-5,0.0529340922159572,0.0116357978393905));
#7450=CARTESIAN_POINT('',(-8.12506199994636E-5,0.0519321483087437,0.0104194415588719));
#7451=CARTESIAN_POINT('',(-8.43928020608055E-5,0.0506415015783407,0.00944944180385272));
#7452=CARTESIAN_POINT('',(-8.76647539264997E-5,0.0492073273028014,0.00882504461561704));
#7453=CARTESIAN_POINT('',(-7.87045304633841E-5,0.0529340922159572,0.0116357978393905));
#7454=CARTESIAN_POINT('',(-8.76647539263809E-5,0.0492073273028014,0.00882504461561705));
#7455=CARTESIAN_POINT('',(0.,0.06842,0.0116357978393905));
#7456=CARTESIAN_POINT('',(-0.0132493773070601,0.060402922273412,0.0116357978393905));
#7457=CARTESIAN_POINT('',(-0.0132493773070601,0.060402922273412,0.0116357978393905));
#7458=CARTESIAN_POINT('',(-0.0129415944843387,0.0593692724324228,0.0113058495927241));
#7459=CARTESIAN_POINT('',(-0.0123626737236229,0.057352839828672,0.0104792531774307));
#7460=CARTESIAN_POINT('',(-0.0113509423413671,0.0532843354740351,0.00880854902741569));
#7461=CARTESIAN_POINT('',(-0.0108078930523591,0.0500332694111306,0.00799377303329642));
#7462=CARTESIAN_POINT('',(-0.0105921890504176,0.0477738844607519,0.00799377303329589));
#7463=CARTESIAN_POINT('',(-0.0070565442830717,0.0463143052920532,0.00799377303329589));
#7464=CARTESIAN_POINT('',(-0.00617530299378738,0.0472946724703008,0.00799377303329588));
#7465=CARTESIAN_POINT('',(-0.00398690985736601,0.0487289177719897,0.0084390364647571));
#7466=CARTESIAN_POINT('',(-0.00140037055543677,0.0491971093619506,0.00881798832068766));
#7467=CARTESIAN_POINT('',(-8.76647097150039E-5,0.0492073466820214,0.00882505305278234));
#7468=CARTESIAN_POINT('',(0.03650000008,0.0452155333197847,0.0179937730332959));
#7469=CARTESIAN_POINT('',(7.87045304628983E-5,0.0529340922159572,0.0116357978393905));
#7470=CARTESIAN_POINT('',(8.12506199994635E-5,0.0519321483087437,0.0104194415588719));
#7471=CARTESIAN_POINT('',(8.43928020602378E-5,0.0506415015783407,0.00944944180385273));
#7472=CARTESIAN_POINT('',(8.76647539255388E-5,0.0492073273028014,0.00882504461561705));
#7473=CARTESIAN_POINT('',(7.8704530463384E-5,0.0529340922159572,0.0116357978393905));
#7474=CARTESIAN_POINT('',(8.76647539276827E-5,0.0492073273028014,0.00882504461561705));
#7475=CARTESIAN_POINT('',(0.03650000008,0.0529340922159572,0.0116357978393905));
#7476=CARTESIAN_POINT('',(-8.76647539264086E-5,0.0492073273028014,0.00882504461561705));
#7477=CARTESIAN_POINT('',(-2.92215846419373E-5,0.0492078331572327,0.00882526484971964));
#7478=CARTESIAN_POINT('',(2.92215846421801E-5,0.0492078331572327,0.00882526484971964));
#7479=CARTESIAN_POINT('',(8.76647539259437E-5,0.0492073273028014,0.00882504461561705));
#7480=CARTESIAN_POINT('',(0.,0.06842,0.0179937730332959));
#7481=CARTESIAN_POINT('',(0.0105921890504172,0.0477738844607486,0.00799377303329589));
#7482=CARTESIAN_POINT('',(0.0108078930523586,0.0500332694111275,0.00799377303329589));
#7483=CARTESIAN_POINT('',(0.0113509423413671,0.0532843354740351,0.0088085490274156));
#7484=CARTESIAN_POINT('',(0.0123626737236227,0.0573528398286717,0.0104792531774306));
#7485=CARTESIAN_POINT('',(0.0129415944843386,0.0593692724324227,0.0113058495927241));
#7486=CARTESIAN_POINT('',(0.0132493773070601,0.060402922273412,0.0116357978393905));
#7487=CARTESIAN_POINT('',(0.0132493773070601,0.060402922273412,0.0116357978393905));
#7488=CARTESIAN_POINT('',(0.,0.06842,0.0116357978393905));
#7489=CARTESIAN_POINT('',(8.76647097150728E-5,0.0492073466820214,0.00882505305278234));
#7490=CARTESIAN_POINT('',(0.00140037055543682,0.0491971093619506,0.00881798832068765));
#7491=CARTESIAN_POINT('',(0.00398690985736599,0.0487289177719897,0.0084390364647571));
#7492=CARTESIAN_POINT('',(0.00617530299378739,0.0472946724703008,0.00799377303329588));
#7493=CARTESIAN_POINT('',(0.0070565442830717,0.0463143052920532,0.00799377303329589));
#7494=CARTESIAN_POINT('',(0.,-0.0684221052,-0.0179937730332959));
#7495=CARTESIAN_POINT('',(0.0150966619928098,-0.0333889120212215,-0.00799377303329591));
#7496=CARTESIAN_POINT('',(0.0156245563131541,-0.0355097001088308,-0.00799377303329591));
#7497=CARTESIAN_POINT('',(0.0171293719837654,-0.0395124805465279,-0.00887297982396414));
#7498=CARTESIAN_POINT('',(0.0192473600818881,-0.0430417062190822,-0.0102455541943977));
#7499=CARTESIAN_POINT('',(0.020465779284996,-0.044769026527585,-0.0107267070030277));
#7500=CARTESIAN_POINT('',(0.020465779284996,-0.044769026527585,-0.0107267070030277));
#7501=CARTESIAN_POINT('',(0.,-0.0684221052,-0.0107267070030269));
#7502=CARTESIAN_POINT('',(-0.0204657792849939,-0.044769026527582,-0.0107267070030269));
#7503=CARTESIAN_POINT('',(-0.0204657792849939,-0.044769026527582,-0.0107267070030269));
#7504=CARTESIAN_POINT('',(-0.0192473600818865,-0.0430417062190796,-0.0102455541943968));
#7505=CARTESIAN_POINT('',(-0.0171293719837647,-0.0395124805465262,-0.00887297982396364));
#7506=CARTESIAN_POINT('',(-0.0156245563131539,-0.0355097001088302,-0.00799377303329591));
#7507=CARTESIAN_POINT('',(-0.0150966619928098,-0.0333889120212215,-0.00799377303329591));
#7508=CARTESIAN_POINT('',(-0.00223898065795575,-0.0303403406237615,-0.00799377303329591));
#7509=CARTESIAN_POINT('',(-0.000746326885985252,-0.0305800173967141,-0.00799377303329591));
#7510=CARTESIAN_POINT('',(0.000746326885985252,-0.0305800173967141,-0.0079937730332959));
#7511=CARTESIAN_POINT('',(0.00223898065795575,-0.0303403406237615,-0.0079937730332959));
#7512=CARTESIAN_POINT('',(0.,-0.0684221052,0.0179937730332959));
#7513=CARTESIAN_POINT('',(-0.0150966619928097,-0.0333889120212214,0.00799377303329588));
#7514=CARTESIAN_POINT('',(-0.015624556313154,-0.0355097001088307,0.00799377303329588));
#7515=CARTESIAN_POINT('',(-0.0171293719837654,-0.0395124805465279,0.00887297982396415));
#7516=CARTESIAN_POINT('',(-0.019247360081888,-0.0430417062190821,0.0102455541943978));
#7517=CARTESIAN_POINT('',(-0.020465779284996,-0.0447690265275849,0.0107267070030278));
#7518=CARTESIAN_POINT('',(-0.020465779284996,-0.0447690265275849,0.0107267070030277));
#7519=CARTESIAN_POINT('',(0.,-0.0684221052,0.0107267070030269));
#7520=CARTESIAN_POINT('',(0.0204657792849938,-0.0447690265275819,0.0107267070030269));
#7521=CARTESIAN_POINT('',(0.0204657792849938,-0.0447690265275819,0.0107267070030269));
#7522=CARTESIAN_POINT('',(0.0192473600818866,-0.0430417062190798,0.0102455541943969));
#7523=CARTESIAN_POINT('',(0.0171293719837646,-0.0395124805465257,0.00887297982396374));
#7524=CARTESIAN_POINT('',(0.0156245563131549,-0.0355097001088332,0.00799377303329635));
#7525=CARTESIAN_POINT('',(0.0150966619928105,-0.0333889120212248,0.00799377303329588));
#7526=CARTESIAN_POINT('',(0.00223898065795594,-0.0303403406237614,0.00799377303329588));
#7527=CARTESIAN_POINT('',(0.000746326885985315,-0.0305800173967141,0.00799377303329588));
#7528=CARTESIAN_POINT('',(-0.000746326885985315,-0.0305800173967141,0.00799377303329587));
#7529=CARTESIAN_POINT('',(-0.00223898065795594,-0.0303403406237614,0.00799377303329587));
#7530=CARTESIAN_POINT('',(0.,-0.0180515951329767,0.0026));
#7531=CARTESIAN_POINT('',(-0.0114910488,-0.0180515951329767,0.0026));
#7532=CARTESIAN_POINT('',(-0.0114910488,-0.0180515951329767,0.00233582142178957));
#7533=CARTESIAN_POINT('',(-0.0112753897480323,-0.018057692716622,0.00181816981976291));
#7534=CARTESIAN_POINT('',(-0.010751370193641,-0.0180720491888493,0.00159999999999997));
#7535=CARTESIAN_POINT('',(-0.0104910129546955,-0.018079019727579,0.0016));
#7536=CARTESIAN_POINT('',(0.0114910488,-0.0180515951329767,0.0026));
#7537=CARTESIAN_POINT('',(0.0114910488,-0.0180515951329767,0.00233582142178958));
#7538=CARTESIAN_POINT('',(0.0112753897480323,-0.0180576927166228,0.00181816981976292));
#7539=CARTESIAN_POINT('',(0.010751370193641,-0.0180720491888478,0.00159999999999997));
#7540=CARTESIAN_POINT('',(0.0104910129546956,-0.018079019727579,0.0016));
#7541=CARTESIAN_POINT('',(0.00944571741540203,0.000530563534951791,0.0026));
#7542=CARTESIAN_POINT('',(0.008207892,0.0403990320215515,0.0026));
#7543=CARTESIAN_POINT('',(0.008207892,0.0403990320215515,0.00233582041202305));
#7544=CARTESIAN_POINT('',(0.00799223219364738,0.0403929152387224,0.00181816659020097));
#7545=CARTESIAN_POINT('',(0.0074682025896938,0.0403787024449846,0.00160000000000004));
#7546=CARTESIAN_POINT('',(0.0072078408582554,0.0403718797522114,0.0016));
#7547=CARTESIAN_POINT('',(-0.00944571741540203,0.000530563534951791,0.0026));
#7548=CARTESIAN_POINT('',(-0.008207892,0.0403990320215515,0.0026));
#7549=CARTESIAN_POINT('',(-0.008207892,0.0403990320215515,0.00233582041202305));
#7550=CARTESIAN_POINT('',(-0.00799223219364738,0.0403929152387224,0.00181816659020097));
#7551=CARTESIAN_POINT('',(-0.0074682025896938,0.0403787024449846,0.00160000000000004));
#7552=CARTESIAN_POINT('',(-0.0072078408582554,0.0403718797522114,0.0016));
#7553=CARTESIAN_POINT('',(0.,0.0403990320215515,0.0026));
#7554=CARTESIAN_POINT('',(0.,0.,0.0130000004));
#7555=CARTESIAN_POINT('',(0.,0.06842,0.0130000004));
#7556=CARTESIAN_POINT('',(0.012,0.06842,0.0130000004));
#7557=CARTESIAN_POINT('',(0.,0.06842,0.0130000004));
#7558=CARTESIAN_POINT('',(0.0122,0.06842,0.0130000004));
#7559=CARTESIAN_POINT('',(0.,0.,-0.0130000004));
#7560=CARTESIAN_POINT('',(0.,0.06842,-0.0130000004));
#7561=CARTESIAN_POINT('',(-0.012,0.06842,-0.0130000004));
#7562=CARTESIAN_POINT('',(0.,0.06842,-0.0130000004));
#7563=CARTESIAN_POINT('',(0.0122,0.06842,-0.0130000004));
#7564=CARTESIAN_POINT('',(0.,-0.0180515951329767,-0.00699377303329591));
#7565=CARTESIAN_POINT('',(-0.00223898065795575,-0.0303403406237615,-0.00699377303329591));
#7566=CARTESIAN_POINT('',(-0.0114910488,-0.0180515951329767,-0.00699377303329591));
#7567=CARTESIAN_POINT('',(-0.0114910488,-0.0180515951329767,-0.0072579473393628));
#7568=CARTESIAN_POINT('',(-0.011706704997243,-0.0180455852288076,-0.00777558982005122));
#7569=CARTESIAN_POINT('',(-0.0122306785725227,-0.018030548260386,-0.00799377303329577));
#7570=CARTESIAN_POINT('',(-0.0124910159490166,-0.0180229475260996,-0.00799377303329591));
#7571=CARTESIAN_POINT('',(-0.00834780990288846,0.055739290033391,-0.0069937730332959));
#7572=CARTESIAN_POINT('',(-0.008207892,0.0403990320215515,-0.0069937730332959));
#7573=CARTESIAN_POINT('',(-0.008207892,0.0403990320215515,-0.00725794661302549));
#7574=CARTESIAN_POINT('',(-0.0084235477697883,0.0404050261404904,-0.00777558759299344));
#7575=CARTESIAN_POINT('',(-0.00894751289069499,0.0404201914761733,-0.00799377303329587));
#7576=CARTESIAN_POINT('',(-0.00920784674600953,0.0404279004413884,-0.0079937730332959));
#7577=CARTESIAN_POINT('',(0.00223898065795575,-0.0303403406237615,-0.00799377303329591));
#7578=CARTESIAN_POINT('',(0.00205973384739524,-0.029356536486291,-0.00799377303329591));
#7579=CARTESIAN_POINT('',(0.00205973384739524,-0.029356536486291,-0.00699377303329591));
#7580=CARTESIAN_POINT('',(0.000748242919122894,-0.0305797097356639,-0.00799377303329591));
#7581=CARTESIAN_POINT('',(0.000715497284703133,-0.0296014532411425,-0.00796255052786754));
#7582=CARTESIAN_POINT('',(0.000686577949441513,-0.0296067222760596,-0.00699377303671879));
#7583=CARTESIAN_POINT('',(-0.000748242919126098,-0.0305797097356639,-0.00799377303329591));
#7584=CARTESIAN_POINT('',(-0.000715497284704723,-0.0296014532411425,-0.00796255052786754));
#7585=CARTESIAN_POINT('',(-0.00068657794944333,-0.0296067222760592,-0.00699377303671879));
#7586=CARTESIAN_POINT('',(-0.00223898065795575,-0.0303403406237615,-0.00799377303329591));
#7587=CARTESIAN_POINT('',(-0.00205973384739524,-0.029356536486291,-0.00799377303329591));
#7588=CARTESIAN_POINT('',(-0.00205973384739524,-0.029356536486291,-0.00699377303329591));
#7589=CARTESIAN_POINT('',(0.00223898065795575,-0.0303403406237615,-0.00699377303329591));
#7590=CARTESIAN_POINT('',(0.,0.0403990320215515,-0.0069937730332959));
#7591=CARTESIAN_POINT('',(-0.0070565442830717,0.0463143052920532,-0.0069937730332959));
#7592=CARTESIAN_POINT('',(0.,-0.0180515951329767,-0.00699377303329591));
#7593=CARTESIAN_POINT('',(0.0114910488,-0.0180515951329767,-0.00699377303329591));
#7594=CARTESIAN_POINT('',(0.0114910488,-0.0180515951329767,-0.00725794733936287));
#7595=CARTESIAN_POINT('',(0.0117067049972432,-0.018045585228809,-0.00777558982005143));
#7596=CARTESIAN_POINT('',(0.0122306785725229,-0.018030548260383,-0.00799377303329588));
#7597=CARTESIAN_POINT('',(0.0124910159490171,-0.0180229475260996,-0.00799377303329591));
#7598=CARTESIAN_POINT('',(-0.0070565442830717,0.0463143052920532,-0.0079937730332959));
#7599=CARTESIAN_POINT('',(-0.00629018600225436,0.0456718918851082,-0.00799377303329591));
#7600=CARTESIAN_POINT('',(-0.00629018600225436,0.0456718918851082,-0.0069937730332959));
#7601=CARTESIAN_POINT('',(-0.00663675715233594,0.0467813119196923,-0.0079937730332959));
#7602=CARTESIAN_POINT('',(-0.00593832363413277,0.0460916412822681,-0.0079723098444523));
#7603=CARTESIAN_POINT('',(-0.00590046854092345,0.0461367999963669,-0.006993773037332));
#7604=CARTESIAN_POINT('',(-0.0056995674399402,0.0476010156616628,-0.00809040380897162));
#7605=CARTESIAN_POINT('',(-0.00516716899465654,0.0468516022761799,-0.00800170584891996));
#7606=CARTESIAN_POINT('',(-0.00503969845558171,0.0469583719208727,-0.00710006688468518));
#7607=CARTESIAN_POINT('',(-0.00343035019733571,0.048822457084395,-0.00851824659842761));
#7608=CARTESIAN_POINT('',(-0.00322701332654168,0.0481104007221522,-0.00828757882417036));
#7609=CARTESIAN_POINT('',(-0.00299842737141113,0.0482019239037002,-0.00757069395613868));
#7610=CARTESIAN_POINT('',(-0.00140299443024509,0.0492029057968726,-0.00882198790030471));
#7611=CARTESIAN_POINT('',(-0.00128861423874107,0.048601413833971,-0.00856090079419736));
#7612=CARTESIAN_POINT('',(-0.00122463996233032,0.0486019331129095,-0.00790480938657816));
#7613=CARTESIAN_POINT('',(-3.88600902706837E-5,0.0492076213378734,-0.00882524260713517));
#7614=CARTESIAN_POINT('',(-3.56761871707623E-5,0.048606846674528,-0.00856365092865193));
#7615=CARTESIAN_POINT('',(-3.3919989452083E-5,0.0486068539322644,-0.00790838956451909));
#7616=CARTESIAN_POINT('',(-7.73280731625782E-5,0.0486067841404136,-0.00790817557838339));
#7617=CARTESIAN_POINT('',(-7.79525636419675E-5,0.0486067680811581,-0.00803052154214757));
#7618=CARTESIAN_POINT('',(-8.02997886509625E-5,0.0486476233580726,-0.00835342390755972));
#7619=CARTESIAN_POINT('',(-8.48435892314036E-5,0.0489650114210101,-0.00871946462590189));
#7620=CARTESIAN_POINT('',(-8.76646190459199E-5,0.0492073271001888,-0.00882504508381696));
#7621=CARTESIAN_POINT('',(0.0114425698213259,0.000642726224631287,-0.00699377303329591));
#7622=CARTESIAN_POINT('',(0.008207892,0.0403990320215515,-0.0069937730332959));
#7623=CARTESIAN_POINT('',(0.008207892,0.0403990320215515,-0.00725794661302555));
#7624=CARTESIAN_POINT('',(0.00842354776978842,0.04040502614049,-0.00777558759299362));
#7625=CARTESIAN_POINT('',(0.00894751289069526,0.0404201914761742,-0.00799377303329597));
#7626=CARTESIAN_POINT('',(0.00920784674600989,0.0404279004413884,-0.0079937730332959));
#7627=CARTESIAN_POINT('',(2.64772969592201E-7,0.0496067633136083,-0.00790830685388911));
#7628=CARTESIAN_POINT('',(8.76646190442611E-5,0.0492073271002133,-0.00882504508376052));
#7629=CARTESIAN_POINT('',(8.48436080713886E-5,0.0489650130516421,-0.00871946530317839));
#7630=CARTESIAN_POINT('',(8.02998525257403E-5,0.0486476250247848,-0.008353427333427));
#7631=CARTESIAN_POINT('',(7.79525723050023E-5,0.0486067681697317,-0.00803052328677894));
#7632=CARTESIAN_POINT('',(7.73280728928411E-5,0.0486067842334127,-0.00790817557840466));
#7633=CARTESIAN_POINT('',(0.,0.0403990320215515,-0.0069937730332959));
#7634=CARTESIAN_POINT('',(0.0070565442830717,0.0463143052920532,-0.0069937730332959));
#7635=CARTESIAN_POINT('',(0.00629018600225436,0.0456718918851082,-0.0069937730332959));
#7636=CARTESIAN_POINT('',(0.00629018600225436,0.0456718918851082,-0.00799377303329591));
#7637=CARTESIAN_POINT('',(0.0070565442830717,0.0463143052920532,-0.0079937730332959));
#7638=CARTESIAN_POINT('',(0.00590046854092339,0.0461367999963669,-0.006993773037332));
#7639=CARTESIAN_POINT('',(0.00593832363413271,0.0460916412822682,-0.0079723098444523));
#7640=CARTESIAN_POINT('',(0.00663675715233588,0.0467813119196924,-0.0079937730332959));
#7641=CARTESIAN_POINT('',(0.0050396984555815,0.0469583719208729,-0.00710006688468504));
#7642=CARTESIAN_POINT('',(0.00516716899465523,0.04685160227618,-0.00800170584891948));
#7643=CARTESIAN_POINT('',(0.00569956743993997,0.0476010156616624,-0.00809040380897139));
#7644=CARTESIAN_POINT('',(0.00299842737141054,0.0482019239037004,-0.00757069395613965));
#7645=CARTESIAN_POINT('',(0.00322701332654435,0.0481104007221538,-0.00828757882417294));
#7646=CARTESIAN_POINT('',(0.00343035019733507,0.0488224570843983,-0.00851824659842906));
#7647=CARTESIAN_POINT('',(0.00122463996232939,0.0486019331129096,-0.00790480938657469));
#7648=CARTESIAN_POINT('',(0.00128861423873465,0.0486014138339637,-0.00856090079418587));
#7649=CARTESIAN_POINT('',(0.00140299443024396,0.0492029057968596,-0.0088219879002991));
#7650=CARTESIAN_POINT('',(3.39199894509637E-5,0.0486068539322645,-0.0079083895645191));
#7651=CARTESIAN_POINT('',(3.56761871695851E-5,0.048606846674528,-0.00856365092865193));
#7652=CARTESIAN_POINT('',(3.88600902694015E-5,0.0492076213378734,-0.00882524260713517));
#7653=CARTESIAN_POINT('',(-0.0479406149651572,-0.0267770382679513,-0.0100000004));
#7654=CARTESIAN_POINT('',(-0.0200162970866488,-0.0452885101813074,-0.0100000004));
#7655=CARTESIAN_POINT('',(-0.03550000008,-0.0578844846861028,-0.0100000004));
#7656=CARTESIAN_POINT('',(-0.0150966619928097,-0.0333889120212215,-0.00799377303329591));
#7657=CARTESIAN_POINT('',(-0.0160769945899837,-0.0331915595474134,-0.00799377303329591));
#7658=CARTESIAN_POINT('',(-0.0160769945899837,-0.0331915595474134,-0.00699377303329591));
#7659=CARTESIAN_POINT('',(-0.0156068158481616,-0.0354384287075173,-0.00799377303329591));
#7660=CARTESIAN_POINT('',(-0.0164617445110731,-0.035102773952805,-0.00790249484159822));
#7661=CARTESIAN_POINT('',(-0.0165074089866533,-0.0353296085680631,-0.00699377303908019));
#7662=CARTESIAN_POINT('',(-0.0170663475656837,-0.039383215844906,-0.00882366076849526));
#7663=CARTESIAN_POINT('',(-0.0175691716233766,-0.0389007355739446,-0.00846666609674932));
#7664=CARTESIAN_POINT('',(-0.0177790331975686,-0.0394032662983781,-0.0079066495412633));
#7665=CARTESIAN_POINT('',(-0.0192020228604743,-0.0429774328463443,-0.0102276505555632));
#7666=CARTESIAN_POINT('',(-0.0195815577937006,-0.0428095980046082,-0.00992665585498258));
#7667=CARTESIAN_POINT('',(-0.0196915521790689,-0.0429887931415983,-0.00945103830350947));
#7668=CARTESIAN_POINT('',(-0.0204657792849939,-0.044769026527582,-0.0107267070030269));
#7669=CARTESIAN_POINT('',(-0.0207883947143825,-0.0446433660335933,-0.0104373351105851));
#7670=CARTESIAN_POINT('',(-0.0208497874735458,-0.04473597622312,-0.0100000004));
#7671=CARTESIAN_POINT('',(-0.0200162970866488,-0.0452885101813074,-0.0100000004));
#7672=CARTESIAN_POINT('',(-0.0150966619928098,-0.0333889120212215,-0.00699377303329591));
#7673=CARTESIAN_POINT('',(-0.0479406149651572,-0.0267770382679513,-0.00699377303329591));
#7674=CARTESIAN_POINT('',(-0.0144904743180211,-0.028655924125519,-0.00699377303329591));
#7675=CARTESIAN_POINT('',(-0.00974560658703515,0.0558178039161666,-0.0069937730332959));
#7676=CARTESIAN_POINT('',(-0.0106041148871086,0.0405336272491669,-0.0069937730332959));
#7677=CARTESIAN_POINT('',(-0.0770011542117716,0.0442631319913884,-0.0069937730332959));
#7678=CARTESIAN_POINT('',(-0.0105921890504172,0.0477738844607486,-0.0069937730332959));
#7679=CARTESIAN_POINT('',(-0.0115907945846862,0.0477210925397055,-0.0069937730332959));
#7680=CARTESIAN_POINT('',(-0.0115907945846862,0.0477210925397055,-0.0079937730332959));
#7681=CARTESIAN_POINT('',(-0.0105921890504172,0.0477738844607486,-0.0079937730332959));
#7682=CARTESIAN_POINT('',(-0.01165154122072,0.0488701684917268,-0.00699377303594161));
#7683=CARTESIAN_POINT('',(-0.0116460760642758,0.0487667902637238,-0.00794865545244461));
#7684=CARTESIAN_POINT('',(-0.0106957683040226,0.0488588221723721,-0.0079937730332959));
#7685=CARTESIAN_POINT('',(-0.0118303126054588,0.0511152954428173,-0.00726680033960579));
#7686=CARTESIAN_POINT('',(-0.0118031703322195,0.0508361592339155,-0.00808736980036333));
#7687=CARTESIAN_POINT('',(-0.0109685466035931,0.0509905050542695,-0.0082419796763848));
#7688=CARTESIAN_POINT('',(-0.0122589931203777,0.054381431806862,-0.00828727294311499));
#7689=CARTESIAN_POINT('',(-0.0122076213027984,0.0540496545607623,-0.0089013378879519));
#7690=CARTESIAN_POINT('',(-0.0115702429201374,0.0541479034369538,-0.00916968204236862));
#7691=CARTESIAN_POINT('',(-0.0128211649345838,0.0574770135698705,-0.00966421320592845));
#7692=CARTESIAN_POINT('',(-0.0127613931441634,0.0571911655524021,-0.010111758697774));
#7693=CARTESIAN_POINT('',(-0.0123263746292068,0.0572218599509659,-0.0104214459159332));
#7694=CARTESIAN_POINT('',(-0.0132893215582587,0.0595090645092476,-0.0106162645372993));
#7695=CARTESIAN_POINT('',(-0.0132467806557753,0.0593347911246909,-0.0110069763062972));
#7696=CARTESIAN_POINT('',(-0.0129239618696845,0.0593100555036758,-0.0112869471314198));
#7697=CARTESIAN_POINT('',(-0.0135575831556229,0.0605538020003774,-0.0110000003200065));
#7698=CARTESIAN_POINT('',(-0.0135257202877438,0.0604297129284592,-0.0113656106861467));
#7699=CARTESIAN_POINT('',(-0.0132493773070656,0.0604029222734306,-0.0116357978393965));
#7700=CARTESIAN_POINT('',(-0.0125890041486941,0.0608025080665215,-0.0110000003200065));
#7701=CARTESIAN_POINT('',(0.0479406149651572,-0.0267770382679513,-0.0100000004));
#7702=CARTESIAN_POINT('',(0.03550000008,-0.0578844846861028,-0.0100000004));
#7703=CARTESIAN_POINT('',(0.0200162970866488,-0.0452885101813074,-0.0100000004));
#7704=CARTESIAN_POINT('',(0.0160769945899837,-0.0331915595474134,-0.00699377303329591));
#7705=CARTESIAN_POINT('',(0.0160769945899837,-0.0331915595474134,-0.00799377303329591));
#7706=CARTESIAN_POINT('',(0.0150966619928097,-0.0333889120212215,-0.00799377303329591));
#7707=CARTESIAN_POINT('',(0.0165074089866533,-0.0353296085680631,-0.00699377303908019));
#7708=CARTESIAN_POINT('',(0.0164617445110731,-0.035102773952805,-0.00790249484159823));
#7709=CARTESIAN_POINT('',(0.0156068158481616,-0.0354384287075173,-0.00799377303329591));
#7710=CARTESIAN_POINT('',(0.0177790331975681,-0.0394032662983772,-0.00790664954127394));
#7711=CARTESIAN_POINT('',(0.0175691716233725,-0.0389007355739614,-0.00846666609676319));
#7712=CARTESIAN_POINT('',(0.0170663475656786,-0.0393832158449129,-0.00882366076850327));
#7713=CARTESIAN_POINT('',(0.01969155217907,-0.0429887931416,-0.00945103830348819));
#7714=CARTESIAN_POINT('',(0.019581557793716,-0.0428095980045924,-0.00992665585496257));
#7715=CARTESIAN_POINT('',(0.0192020228604844,-0.0429774328463306,-0.0102276505555471));
#7716=CARTESIAN_POINT('',(0.0208497874735458,-0.04473597622312,-0.0100000004));
#7717=CARTESIAN_POINT('',(0.0207883947143824,-0.0446433660335932,-0.0104373351105851));
#7718=CARTESIAN_POINT('',(0.0204657792849938,-0.0447690265275819,-0.0107267070030269));
#7719=CARTESIAN_POINT('',(0.0200162970866488,-0.0452885101813074,-0.0100000004));
#7720=CARTESIAN_POINT('',(0.0150966619928098,-0.0333889120212215,-0.00699377303329591));
#7721=CARTESIAN_POINT('',(0.0479406149651572,-0.0267770382679513,-0.00699377303329591));
#7722=CARTESIAN_POINT('',(0.0144904743180211,-0.028655924125519,-0.00699377303329591));
#7723=CARTESIAN_POINT('',(0.0128403665054726,0.000721240107406931,-0.00699377303329591));
#7724=CARTESIAN_POINT('',(0.0106041148871086,0.0405336272491669,-0.0069937730332959));
#7725=CARTESIAN_POINT('',(0.0770011542117716,0.0442631319913884,-0.0069937730332959));
#7726=CARTESIAN_POINT('',(0.0105921890504172,0.0477738844607486,-0.0069937730332959));
#7727=CARTESIAN_POINT('',(0.0105921890504172,0.0477738844607486,-0.0079937730332959));
#7728=CARTESIAN_POINT('',(0.0115907945846862,0.0477210925397055,-0.0079937730332959));
#7729=CARTESIAN_POINT('',(0.0115907945846862,0.0477210925397055,-0.0069937730332959));
#7730=CARTESIAN_POINT('',(0.0106957683040225,0.0488588221723706,-0.0079937730332959));
#7731=CARTESIAN_POINT('',(0.0116460760642757,0.0487667902637224,-0.00794865545244467));
#7732=CARTESIAN_POINT('',(0.01165154122072,0.0488701684917252,-0.00699377303594161));
#7733=CARTESIAN_POINT('',(0.0109685466035914,0.0509905050542603,-0.00824197967638226));
#7734=CARTESIAN_POINT('',(0.0118031703322181,0.0508361592339046,-0.00808736980036114));
#7735=CARTESIAN_POINT('',(0.0118303126054573,0.0511152954428084,-0.0072668003396034));
#7736=CARTESIAN_POINT('',(0.0115702429201392,0.0541479034369613,-0.00916968204237201));
#7737=CARTESIAN_POINT('',(0.0122076213028006,0.0540496545607744,-0.00890133788795471));
#7738=CARTESIAN_POINT('',(0.01225899312038,0.0543814318068674,-0.00828727294311731));
#7739=CARTESIAN_POINT('',(0.0123263746291898,0.0572218599508923,-0.0104214459159037));
#7740=CARTESIAN_POINT('',(0.0127613931441495,0.0571911655523188,-0.0101117586977502));
#7741=CARTESIAN_POINT('',(0.0128211649345674,0.0574770135698036,-0.00966421320590118));
#7742=CARTESIAN_POINT('',(0.0129239618697091,0.0593100555037898,-0.0112869471314648));
#7743=CARTESIAN_POINT('',(0.0132467806557945,0.0593347911248174,-0.0110069763063276));
#7744=CARTESIAN_POINT('',(0.0132893215582847,0.0595090645093479,-0.0106162645373376));
#7745=CARTESIAN_POINT('',(0.0132493773070601,0.060402922273412,-0.0116357978393905));
#7746=CARTESIAN_POINT('',(0.0135257202877391,0.0604297129284408,-0.0113656106861407));
#7747=CARTESIAN_POINT('',(0.0135575831556184,0.0605538020003596,-0.01100000032));
#7748=CARTESIAN_POINT('',(0.0125890041486895,0.0608025080665035,-0.01100000032));
#7749=CARTESIAN_POINT('',(0.,-0.0180515951329767,0.00699377303329588));
#7750=CARTESIAN_POINT('',(0.00223898065795594,-0.0303403406237614,0.00699377303329588));
#7751=CARTESIAN_POINT('',(0.0114910488,-0.0180515951329767,0.00699377303329588));
#7752=CARTESIAN_POINT('',(0.0114910488,-0.0180515951329767,0.00725794733936277));
#7753=CARTESIAN_POINT('',(0.0117067049972431,-0.0180455852288112,0.00777558982005119));
#7754=CARTESIAN_POINT('',(0.0122306785725225,-0.0180305482603787,0.00799377303329574));
#7755=CARTESIAN_POINT('',(0.0124910159490166,-0.0180229475260995,0.00799377303329588));
#7756=CARTESIAN_POINT('',(0.00857740346184122,0.0516517948789017,0.00699377303329589));
#7757=CARTESIAN_POINT('',(0.008207892,0.0403990320215515,0.00699377303329589));
#7758=CARTESIAN_POINT('',(0.008207892,0.0403990320215515,0.00725794661302549));
#7759=CARTESIAN_POINT('',(0.00842354776978831,0.0404050261404905,0.00777558759299344));
#7760=CARTESIAN_POINT('',(0.008947512890695,0.0404201914761739,0.00799377303329587));
#7761=CARTESIAN_POINT('',(0.00920784674600956,0.0404279004413884,0.00799377303329589));
#7762=CARTESIAN_POINT('',(-0.00223898065795594,-0.0303403406237614,0.00799377303329588));
#7763=CARTESIAN_POINT('',(-0.00205973384739541,-0.029356536486291,0.00799377303329588));
#7764=CARTESIAN_POINT('',(-0.00205973384739541,-0.029356536486291,0.00699377303329588));
#7765=CARTESIAN_POINT('',(-0.000748242919122951,-0.0305797097356955,0.00799377303329588));
#7766=CARTESIAN_POINT('',(-0.000715497284706645,-0.0296014532411807,0.00796255052794581));
#7767=CARTESIAN_POINT('',(-0.000686577949433335,-0.0296067222760611,0.00699377303680561));
#7768=CARTESIAN_POINT('',(0.00074824291912353,-0.0305797097356876,0.00799377303329588));
#7769=CARTESIAN_POINT('',(0.000715497284696222,-0.0296014532411735,0.00796255052796054));
#7770=CARTESIAN_POINT('',(0.000686577949435276,-0.0296067222760607,0.00699377303680561));
#7771=CARTESIAN_POINT('',(0.00223898065795595,-0.0303403406237614,0.00799377303329588));
#7772=CARTESIAN_POINT('',(0.00205973384739542,-0.029356536486291,0.00799377303329588));
#7773=CARTESIAN_POINT('',(0.00205973384739542,-0.029356536486291,0.00699377303329588));
#7774=CARTESIAN_POINT('',(-0.00223898065795594,-0.0303403406237614,0.00699377303329588));
#7775=CARTESIAN_POINT('',(0.,0.0403990320215515,0.00699377303329589));
#7776=CARTESIAN_POINT('',(0.0070565442830717,0.0463143052920532,0.00699377303329589));
#7777=CARTESIAN_POINT('',(0.,-0.0180515951329767,0.00699377303329588));
#7778=CARTESIAN_POINT('',(-0.0114910488,-0.0180515951329767,0.00699377303329588));
#7779=CARTESIAN_POINT('',(-0.0114910488,-0.0180515951329767,0.00725794733936284));
#7780=CARTESIAN_POINT('',(-0.0117067049972432,-0.0180455852288116,0.00777558982005139));
#7781=CARTESIAN_POINT('',(-0.0122306785725228,-0.0180305482603778,0.00799377303329584));
#7782=CARTESIAN_POINT('',(-0.012491015949017,-0.0180229475260996,0.00799377303329588));
#7783=CARTESIAN_POINT('',(0.0070565442830717,0.0463143052920532,0.00799377303329589));
#7784=CARTESIAN_POINT('',(0.00629018600225436,0.0456718918851082,0.0079937730332959));
#7785=CARTESIAN_POINT('',(0.00629018600225436,0.0456718918851082,0.00699377303329589));
#7786=CARTESIAN_POINT('',(0.00663675715233699,0.0467813119196925,0.00799377303329589));
#7787=CARTESIAN_POINT('',(0.00593832363413206,0.0460916412822597,0.00797230984445771));
#7788=CARTESIAN_POINT('',(0.00590046854092382,0.0461367999963664,0.00699377303733907));
#7789=CARTESIAN_POINT('',(0.00569956743993915,0.0476010156616633,0.00809040380897171));
#7790=CARTESIAN_POINT('',(0.00516716899465536,0.0468516022761816,0.00800170584891698));
#7791=CARTESIAN_POINT('',(0.00503969845558102,0.0469583719208734,0.00710006688468222));
#7792=CARTESIAN_POINT('',(0.00343035019733497,0.0488224570843953,0.00851824659842775));
#7793=CARTESIAN_POINT('',(0.00322701332654366,0.0481104007221627,0.00828757882417505));
#7794=CARTESIAN_POINT('',(0.00299842737141029,0.0482019239037006,0.00757069395613992));
#7795=CARTESIAN_POINT('',(0.00140299443024176,0.0492029057968742,0.00882198790030551));
#7796=CARTESIAN_POINT('',(0.00128861423873263,0.0486014138339194,0.00856090079418309));
#7797=CARTESIAN_POINT('',(0.00122463996232749,0.0486019331129098,0.00790480938658279));
#7798=CARTESIAN_POINT('',(3.88600902680932E-5,0.0492076213378734,0.00882524260713517));
#7799=CARTESIAN_POINT('',(3.56761871683841E-5,0.048606846674528,0.00856365092865193));
#7800=CARTESIAN_POINT('',(3.39199894498218E-5,0.0486068539322645,0.00790838956451909));
#7801=CARTESIAN_POINT('',(7.73286032330566E-5,0.0486066725565947,0.00790817556294355));
#7802=CARTESIAN_POINT('',(7.79535025252851E-5,0.0486066544098561,0.00803061290174059));
#7803=CARTESIAN_POINT('',(8.0300967418879E-5,0.0486475761391194,0.00835362636492919));
#7804=CARTESIAN_POINT('',(8.48436697596153E-5,0.0489649915149441,0.00871960415239467));
#7805=CARTESIAN_POINT('',(8.76638406754314E-5,0.0492072689642466,0.00882517851789361));
#7806=CARTESIAN_POINT('',(-0.0114425698213259,0.000642726224631286,0.00699377303329588));
#7807=CARTESIAN_POINT('',(-0.008207892,0.0403990320215515,0.00699377303329589));
#7808=CARTESIAN_POINT('',(-0.008207892,0.0403990320215515,0.00725794661302554));
#7809=CARTESIAN_POINT('',(-0.00842354776978844,0.0404050261404894,0.0077755875929936));
#7810=CARTESIAN_POINT('',(-0.0089475128906952,0.0404201914761762,0.00799377303329595));
#7811=CARTESIAN_POINT('',(-0.00920784674600988,0.0404279004413884,0.00799377303329589));
#7812=CARTESIAN_POINT('',(-5.61597199378756E-9,0.0496067442138064,0.00790829977384746));
#7813=CARTESIAN_POINT('',(-8.76638410861103E-5,0.0492072689878249,0.00882517846382129));
#7814=CARTESIAN_POINT('',(-8.48436494395307E-5,0.0489649897645646,0.00871960336263682));
#7815=CARTESIAN_POINT('',(-8.03009008679873E-5,0.0486475743651198,0.00835362258293446));
#7816=CARTESIAN_POINT('',(-7.79534925679463E-5,0.0486066543685292,0.00803061098119678));
#7817=CARTESIAN_POINT('',(-7.73286030826419E-5,0.0486066725101695,0.00790817556293302));
#7818=CARTESIAN_POINT('',(0.,0.0403990320215515,0.00699377303329589));
#7819=CARTESIAN_POINT('',(-0.0070565442830717,0.0463143052920532,0.00699377303329589));
#7820=CARTESIAN_POINT('',(-0.00629018600225436,0.0456718918851082,0.00699377303329589));
#7821=CARTESIAN_POINT('',(-0.00629018600225436,0.0456718918851082,0.0079937730332959));
#7822=CARTESIAN_POINT('',(-0.0070565442830717,0.0463143052920532,0.00799377303329589));
#7823=CARTESIAN_POINT('',(-0.00590046854092381,0.0461367999963664,0.00699377303733907));
#7824=CARTESIAN_POINT('',(-0.00593832363413165,0.0460916412822597,0.00797230984445853));
#7825=CARTESIAN_POINT('',(-0.00663675715233699,0.0467813119196925,0.00799377303329589));
#7826=CARTESIAN_POINT('',(-0.00503969845558102,0.0469583719208734,0.00710006688468207));
#7827=CARTESIAN_POINT('',(-0.00516716899465555,0.0468516022761816,0.0080017058489165));
#7828=CARTESIAN_POINT('',(-0.00569956743993915,0.0476010156616632,0.00809040380897169));
#7829=CARTESIAN_POINT('',(-0.00299842737141019,0.0482019239037006,0.00757069395614071));
#7830=CARTESIAN_POINT('',(-0.00322701332654346,0.0481104007221627,0.00828757882417575));
#7831=CARTESIAN_POINT('',(-0.00343035019733485,0.0488224570843956,0.00851824659842788));
#7832=CARTESIAN_POINT('',(-0.00122463996232772,0.0486019331129098,0.00790480938657932));
#7833=CARTESIAN_POINT('',(-0.00128861423873286,0.0486014138339194,0.00856090079418102));
#7834=CARTESIAN_POINT('',(-0.00140299443024203,0.049202905796873,0.00882198790030496));
#7835=CARTESIAN_POINT('',(-3.39199894497602E-5,0.0486068539322645,0.00790838956451909));
#7836=CARTESIAN_POINT('',(-3.56761871683194E-5,0.048606846674528,0.00856365092865193));
#7837=CARTESIAN_POINT('',(-3.88600902680227E-5,0.0492076213378734,0.00882524260713517));
#7838=CARTESIAN_POINT('',(0.0479406149651572,-0.0267770382679513,0.0100000004));
#7839=CARTESIAN_POINT('',(0.0200162970866488,-0.0452885101813074,0.0100000004));
#7840=CARTESIAN_POINT('',(0.03550000008,-0.0578844846861028,0.0100000004));
#7841=CARTESIAN_POINT('',(0.0150966619928104,-0.0333889120212244,0.00799377303329588));
#7842=CARTESIAN_POINT('',(0.0160769945899842,-0.0331915595474162,0.00799377303329574));
#7843=CARTESIAN_POINT('',(0.0160769945899843,-0.0331915595474164,0.00699377303329588));
#7844=CARTESIAN_POINT('',(0.0156068158482343,-0.0354384287074729,0.00799377303329628));
#7845=CARTESIAN_POINT('',(0.0164617445111704,-0.0351027739527766,0.00790249484173019));
#7846=CARTESIAN_POINT('',(0.016507408986648,-0.0353296085680356,0.0069937730392069));
#7847=CARTESIAN_POINT('',(0.0170663475656315,-0.039383215844924,0.00882366076850159));
#7848=CARTESIAN_POINT('',(0.0175691716233034,-0.0389007355739478,0.00846666609668826));
#7849=CARTESIAN_POINT('',(0.0177790331975587,-0.0394032662983737,0.0079066495412027));
#7850=CARTESIAN_POINT('',(0.0192020228605085,-0.0429774328463579,0.0102276505555518));
#7851=CARTESIAN_POINT('',(0.0195815577937507,-0.0428095980046108,0.00992665585498373));
#7852=CARTESIAN_POINT('',(0.0196915521790964,-0.0429887931416397,0.00945103830350577));
#7853=CARTESIAN_POINT('',(0.0204657792849938,-0.0447690265275819,0.0107267070030269));
#7854=CARTESIAN_POINT('',(0.0207883947143824,-0.0446433660335932,0.0104373351105851));
#7855=CARTESIAN_POINT('',(0.0208497874735457,-0.04473597622312,0.0100000004));
#7856=CARTESIAN_POINT('',(0.0200162970866488,-0.0452885101813074,0.0100000004));
#7857=CARTESIAN_POINT('',(0.0150966619928104,-0.033388912021225,0.00699377303329588));
#7858=CARTESIAN_POINT('',(0.0479406149651572,-0.0267770382679513,0.00699377303329588));
#7859=CARTESIAN_POINT('',(0.0144904743180211,-0.028655924125519,0.00699377303329588));
#7860=CARTESIAN_POINT('',(0.00997520014598791,0.0517303087616774,0.00699377303329589));
#7861=CARTESIAN_POINT('',(0.0106041148871086,0.0405336272491669,0.00699377303329589));
#7862=CARTESIAN_POINT('',(0.0770011542117716,0.0442631319913884,0.00699377303329589));
#7863=CARTESIAN_POINT('',(0.0105921890504172,0.0477738844607486,0.00699377303329589));
#7864=CARTESIAN_POINT('',(0.0115907945846862,0.0477210925397055,0.00699377303329589));
#7865=CARTESIAN_POINT('',(0.0115907945846862,0.0477210925397055,0.00799377303329589));
#7866=CARTESIAN_POINT('',(0.0105921890504172,0.0477738844607486,0.00799377303329589));
#7867=CARTESIAN_POINT('',(0.0116515412207203,0.0488701684917309,0.00699377303595376));
#7868=CARTESIAN_POINT('',(0.0116460760642758,0.0487667902637238,0.0079486554524551));
#7869=CARTESIAN_POINT('',(0.0106957683040226,0.0488588221723761,0.00799377303329589));
#7870=CARTESIAN_POINT('',(0.0118303126054586,0.0511152954428151,0.00726680033959949));
#7871=CARTESIAN_POINT('',(0.0118031703322206,0.0508361592339147,0.00808736980035808));
#7872=CARTESIAN_POINT('',(0.0109685466035936,0.0509905050542671,0.00824197967638395));
#7873=CARTESIAN_POINT('',(0.012258993120378,0.0543814318068636,0.00828727294311878));
#7874=CARTESIAN_POINT('',(0.0122076213027949,0.054049654560765,0.008901337887955));
#7875=CARTESIAN_POINT('',(0.0115702429201356,0.0541479034369561,0.0091696820423716));
#7876=CARTESIAN_POINT('',(0.0128211649345827,0.0574770135698663,0.00966421320591958));
#7877=CARTESIAN_POINT('',(0.0127613931441757,0.0571911655523929,0.0101117586977671));
#7878=CARTESIAN_POINT('',(0.0123263746292134,0.057221859950959,0.0104214459159221));
#7879=CARTESIAN_POINT('',(0.0132893215582609,0.0595090645092564,0.0106162645373174));
#7880=CARTESIAN_POINT('',(0.0132467806557497,0.0593347911247093,0.0110069763063105));
#7881=CARTESIAN_POINT('',(0.0129239618696705,0.0593100555036904,0.0112869471314436));
#7882=CARTESIAN_POINT('',(0.0135575831556229,0.0605538020003774,0.0110000003200065));
#7883=CARTESIAN_POINT('',(0.0135257202877438,0.0604297129284592,0.0113656106861467));
#7884=CARTESIAN_POINT('',(0.0132493773070656,0.0604029222734306,0.0116357978393965));
#7885=CARTESIAN_POINT('',(0.0125890041486941,0.0608025080665215,0.0110000003200065));
#7886=CARTESIAN_POINT('',(-0.0479406149651572,-0.0267770382679513,0.0100000004));
#7887=CARTESIAN_POINT('',(-0.0200162970866488,-0.0452885101813074,0.0100000004));
#7888=CARTESIAN_POINT('',(-0.03550000008,-0.0578844846861028,0.0100000004));
#7889=CARTESIAN_POINT('',(-0.0160769945899836,-0.0331915595474134,0.00699377303329588));
#7890=CARTESIAN_POINT('',(-0.0160769945899836,-0.0331915595474134,0.00799377303329588));
#7891=CARTESIAN_POINT('',(-0.0150966619928097,-0.0333889120212214,0.00799377303329588));
#7892=CARTESIAN_POINT('',(-0.0165074089866394,-0.0353296085679943,0.00699377303920885));
#7893=CARTESIAN_POINT('',(-0.0164617445112181,-0.0351027739527186,0.0079024948417222));
#7894=CARTESIAN_POINT('',(-0.0156068158483019,-0.0354384287074471,0.00799377303329588));
#7895=CARTESIAN_POINT('',(-0.0177790331975661,-0.0394032662983982,0.00790664954120865));
#7896=CARTESIAN_POINT('',(-0.0175691716232746,-0.0389007355739849,0.00846666609669959));
#7897=CARTESIAN_POINT('',(-0.0170663475655921,-0.0393832158449445,0.00882366076851098));
#7898=CARTESIAN_POINT('',(-0.0196915521790878,-0.0429887931416268,0.00945103830349017));
#7899=CARTESIAN_POINT('',(-0.0195815577937629,-0.0428095980045893,0.00992665585496803));
#7900=CARTESIAN_POINT('',(-0.0192020228605171,-0.0429774328463374,0.0102276505555318));
#7901=CARTESIAN_POINT('',(-0.0208497874735458,-0.04473597622312,0.0100000004));
#7902=CARTESIAN_POINT('',(-0.0207883947143824,-0.0446433660335932,0.0104373351105851));
#7903=CARTESIAN_POINT('',(-0.0204657792849938,-0.0447690265275819,0.0107267070030269));
#7904=CARTESIAN_POINT('',(-0.0200162970866488,-0.0452885101813074,0.0100000004));
#7905=CARTESIAN_POINT('',(-0.0150966619928097,-0.0333889120212214,0.00699377303329588));
#7906=CARTESIAN_POINT('',(-0.0479406149651572,-0.0267770382679513,0.00699377303329588));
#7907=CARTESIAN_POINT('',(-0.0144904743180211,-0.028655924125519,0.00699377303329588));
#7908=CARTESIAN_POINT('',(-0.0128403665054726,0.00072124010740693,0.00699377303329588));
#7909=CARTESIAN_POINT('',(-0.0106041148871086,0.0405336272491669,0.00699377303329589));
#7910=CARTESIAN_POINT('',(-0.0770011542117716,0.0442631319913884,0.00699377303329589));
#7911=CARTESIAN_POINT('',(-0.0105921890504174,0.0477738844607517,0.00699377303329589));
#7912=CARTESIAN_POINT('',(-0.0105921890504175,0.0477738844607515,0.00799377303329589));
#7913=CARTESIAN_POINT('',(-0.0115907945846863,0.0477210925397084,0.00799377303329577));
#7914=CARTESIAN_POINT('',(-0.0115907945846864,0.0477210925397086,0.00699377303329589));
#7915=CARTESIAN_POINT('',(-0.0106957683040308,0.0488588221723772,0.00799377303329611));
#7916=CARTESIAN_POINT('',(-0.0116460760642879,0.0487667902636878,0.00794865545245672));
#7917=CARTESIAN_POINT('',(-0.0116515412207195,0.0488701684917165,0.00699377303595376));
#7918=CARTESIAN_POINT('',(-0.0109685466035879,0.0509905050542611,0.00824197967638324));
#7919=CARTESIAN_POINT('',(-0.0118031703322129,0.0508361592339223,0.00808736980035708));
#7920=CARTESIAN_POINT('',(-0.011830312605458,0.0511152954428164,0.007266800339599));
#7921=CARTESIAN_POINT('',(-0.011570242920141,0.0541479034369613,0.00916968204237088));
#7922=CARTESIAN_POINT('',(-0.012207621302802,0.0540496545607705,0.00890133788795375));
#7923=CARTESIAN_POINT('',(-0.0122589931203798,0.054381431806866,0.00828727294311737));
#7924=CARTESIAN_POINT('',(-0.0123263746291878,0.0572218599508996,0.0104214459159101));
#7925=CARTESIAN_POINT('',(-0.0127613931441502,0.0571911655523285,0.0101117586977604));
#7926=CARTESIAN_POINT('',(-0.0128211649345689,0.05747701356981,0.00966421320590858));
#7927=CARTESIAN_POINT('',(-0.0129239618697132,0.0593100555037755,0.0112869471314516));
#7928=CARTESIAN_POINT('',(-0.0132467806557926,0.0593347911248004,0.0110069763063061));
#7929=CARTESIAN_POINT('',(-0.0132893215582819,0.0595090645093368,0.0106162645373216));
#7930=CARTESIAN_POINT('',(-0.0132493773070601,0.060402922273412,0.0116357978393905));
#7931=CARTESIAN_POINT('',(-0.0135257202877391,0.0604297129284408,0.0113656106861407));
#7932=CARTESIAN_POINT('',(-0.0135575831556184,0.0605538020003596,0.01100000032));
#7933=CARTESIAN_POINT('',(-0.0125890041486895,0.0608025080665035,0.01100000032));
#7934=CARTESIAN_POINT('',(0.,0.0403990320215515,-0.0026));
#7935=CARTESIAN_POINT('',(0.008207892,0.0403990320215515,-0.0026));
#7936=CARTESIAN_POINT('',(0.008207892,0.0403990320215515,-0.00233582041202306));
#7937=CARTESIAN_POINT('',(0.0079922321936474,0.0403929152387221,-0.001818166590201));
#7938=CARTESIAN_POINT('',(0.00746820258969384,0.0403787024449851,-0.00160000000000006));
#7939=CARTESIAN_POINT('',(0.00720784085825546,0.0403718797522114,-0.0016));
#7940=CARTESIAN_POINT('',(-0.008207892,0.0403990320215515,-0.0026));
#7941=CARTESIAN_POINT('',(-0.008207892,0.0403990320215515,-0.00233582041202305));
#7942=CARTESIAN_POINT('',(-0.00799223219364738,0.0403929152387224,-0.00181816659020097));
#7943=CARTESIAN_POINT('',(-0.0074682025896938,0.0403787024449846,-0.00160000000000004));
#7944=CARTESIAN_POINT('',(-0.0072078408582554,0.0403718797522114,-0.0016));
#7945=CARTESIAN_POINT('',(-0.00944571741540203,0.000530563534951791,-0.0026));
#7946=CARTESIAN_POINT('',(-0.0114910488,-0.0180515951329767,-0.0026));
#7947=CARTESIAN_POINT('',(-0.0114910488,-0.0180515951329767,-0.00233582142178957));
#7948=CARTESIAN_POINT('',(-0.0112753897480323,-0.0180576927166228,-0.00181816981976291));
#7949=CARTESIAN_POINT('',(-0.010751370193641,-0.0180720491888478,-0.00159999999999997));
#7950=CARTESIAN_POINT('',(-0.0104910129546955,-0.018079019727579,-0.0016));
#7951=CARTESIAN_POINT('',(0.00944571741540203,0.000530563534951791,-0.0026));
#7952=CARTESIAN_POINT('',(0.0114910488,-0.0180515951329767,-0.0026));
#7953=CARTESIAN_POINT('',(0.0114910488,-0.0180515951329767,-0.00233582142178957));
#7954=CARTESIAN_POINT('',(0.0112753897480323,-0.018057692716622,-0.00181816981976291));
#7955=CARTESIAN_POINT('',(0.010751370193641,-0.0180720491888493,-0.00159999999999997));
#7956=CARTESIAN_POINT('',(0.0104910129546955,-0.018079019727579,-0.0016));
#7957=CARTESIAN_POINT('',(0.,-0.0180515951329767,-0.0026));
#7958=CARTESIAN_POINT('',(-0.0200162970866488,-0.0452885101813074,0.0100000004));
#7959=CARTESIAN_POINT('',(-0.0200162970866488,-0.0452885101813074,0.0100000004));
#7960=CARTESIAN_POINT('',(0.,-0.0684221052,0.0100000004));
#7961=CARTESIAN_POINT('',(0.0200162970866488,-0.0452885101813074,0.0100000004));
#7962=CARTESIAN_POINT('',(0.0200162970866488,-0.0452885101813074,0.0100000004));
#7963=CARTESIAN_POINT('',(-0.03550000008,-0.0578844846861027,-0.0100000004));
#7964=CARTESIAN_POINT('',(-0.03550000008,-0.0578844846861028,-0.0100000004));
#7965=CARTESIAN_POINT('',(-0.03550000008,-0.0578844846861027,-0.01200000032));
#7966=CARTESIAN_POINT('',(-0.03550000008,-0.0578844846861027,0.0100000004));
#7967=CARTESIAN_POINT('',(-0.03550000008,-0.0578844846861027,0.0100000004));
#7968=CARTESIAN_POINT('',(0.03550000008,-0.0578844846861027,-0.0100000004));
#7969=CARTESIAN_POINT('',(0.03550000008,-0.0578844846861027,-0.0100000004));
#7970=CARTESIAN_POINT('',(0.03550000008,-0.0578844846861027,-0.01200000032));
#7971=CARTESIAN_POINT('',(0.03550000008,-0.0578844846861027,0.0100000004));
#7972=CARTESIAN_POINT('',(0.03550000008,-0.0578844846861027,0.0100000004));
#7973=CARTESIAN_POINT('',(0.0200162970866488,-0.0452885101813074,-0.0100000004));
#7974=CARTESIAN_POINT('',(0.0200162970866488,-0.0452885101813074,-0.0100000004));
#7975=CARTESIAN_POINT('',(0.,-0.0684221052,-0.0100000004));
#7976=CARTESIAN_POINT('',(-0.0200162970866503,-0.0452885101813087,-0.0100000004));
#7977=CARTESIAN_POINT('',(-0.0200162970866488,-0.0452885101813074,-0.0100000004));
#7978=CARTESIAN_POINT('',(0.,0.06842,-0.01100000032));
#7979=CARTESIAN_POINT('',(-0.0135487072274815,0.0641694879715509,-0.01100000032));
#7980=CARTESIAN_POINT('',(0.0135487072274815,0.0641694879715509,-0.01100000032));
#7981=CARTESIAN_POINT('',(0.0770011542117716,0.0442631319913884,-0.01100000032));
#7982=CARTESIAN_POINT('',(0.0125890041486895,0.0608025080665035,-0.01100000032));
#7983=CARTESIAN_POINT('',(-0.0770011542117716,0.0442631319913884,-0.01100000032));
#7984=CARTESIAN_POINT('',(-0.0125890041486895,0.0608025080665034,-0.01100000032));
#7985=CARTESIAN_POINT('',(0.0125890041486895,0.0608025080665035,-0.01100000032));
#7986=CARTESIAN_POINT('',(0.0125890041486895,0.0608025080665035,-0.01100000032));
#7987=CARTESIAN_POINT('',(-0.0125890041486895,0.0608025080665034,-0.01100000032));
#7988=CARTESIAN_POINT('',(-0.0125890041486895,0.0608025080665034,-0.01100000032));
#7989=CARTESIAN_POINT('',(0.,0.06842,-0.01100000032));
#7990=CARTESIAN_POINT('',(7.87045304645721E-5,0.0529340922159572,-0.0116357978393905));
#7991=CARTESIAN_POINT('',(7.82254313897608E-5,0.0531226285545892,-0.0118646802727782));
#7992=CARTESIAN_POINT('',(7.74797395333406E-5,0.0534133411399295,-0.01200000032));
#7993=CARTESIAN_POINT('',(7.67180601915171E-5,0.0537059481055745,-0.01200000032));
#7994=CARTESIAN_POINT('',(0.,0.06842,-0.01100000032));
#7995=CARTESIAN_POINT('',(-7.87045304645737E-5,0.0529340922159572,-0.0116357978393905));
#7996=CARTESIAN_POINT('',(-7.82254313897624E-5,0.0531226285545892,-0.0118646802727782));
#7997=CARTESIAN_POINT('',(-7.74797395310902E-5,0.0534133411399295,-0.01200000032));
#7998=CARTESIAN_POINT('',(-7.67180601914596E-5,0.0537059481055745,-0.01200000032));
#7999=CARTESIAN_POINT('',(0.03650000008,0.0537059481055745,-0.01100000032));
#8000=CARTESIAN_POINT('',(0.,0.06842,-0.01300000032));
#8001=CARTESIAN_POINT('',(0.,0.06842,-0.0120000004));
#8002=CARTESIAN_POINT('',(0.,0.06842,0.0120000004));
#8003=CARTESIAN_POINT('',(0.,0.06842,0.01100000032));
#8004=CARTESIAN_POINT('',(-0.0135487072274815,0.0641694879715509,0.01100000032));
#8005=CARTESIAN_POINT('',(0.0135487072274815,0.0641694879715509,0.01100000032));
#8006=CARTESIAN_POINT('',(0.0770011542117716,0.0442631319913884,0.01100000032));
#8007=CARTESIAN_POINT('',(0.0125890041486819,0.060802508066474,0.01100000032));
#8008=CARTESIAN_POINT('',(-0.0770011542117716,0.0442631319913884,0.01100000032));
#8009=CARTESIAN_POINT('',(-0.0125890041486895,0.0608025080665035,0.01100000032));
#8010=CARTESIAN_POINT('',(0.0125890041486895,0.0608025080665034,0.01100000032));
#8011=CARTESIAN_POINT('',(0.0125890041486895,0.0608025080665034,0.01100000032));
#8012=CARTESIAN_POINT('',(-0.0125890041486895,0.0608025080665035,0.01100000032));
#8013=CARTESIAN_POINT('',(-0.0125890041486895,0.0608025080665035,0.01100000032));
#8014=CARTESIAN_POINT('',(0.,0.06842,0.01100000032));
#8015=CARTESIAN_POINT('',(7.87045304634033E-5,0.0529340922159572,0.0116357978393905));
#8016=CARTESIAN_POINT('',(7.82254313883414E-5,0.0531226285545892,0.0118646802727782));
#8017=CARTESIAN_POINT('',(7.74797395308895E-5,0.0534133411399295,0.01200000032));
#8018=CARTESIAN_POINT('',(7.67180601909946E-5,0.0537059481055745,0.01200000032));
#8019=CARTESIAN_POINT('',(0.,0.06842,0.01100000032));
#8020=CARTESIAN_POINT('',(-7.87045304634164E-5,0.0529340922159572,0.0116357978393905));
#8021=CARTESIAN_POINT('',(-7.82254313883546E-5,0.0531226285545892,0.0118646802727782));
#8022=CARTESIAN_POINT('',(-7.74797395313073E-5,0.0534133411399295,0.01200000032));
#8023=CARTESIAN_POINT('',(-7.67180601908343E-5,0.0537059481055745,0.01200000032));
#8024=CARTESIAN_POINT('',(0.03650000008,0.0537059481055745,0.01100000032));
#8025=CARTESIAN_POINT('',(0.,0.06842,0.01300000032));
#8026=CARTESIAN_POINT('',(0.0434268042445183,-0.0746532949430514,0.0110000004));
#8027=CARTESIAN_POINT('',(0.0434268042445183,-0.0746532949430514,0.0110000004));
#8028=CARTESIAN_POINT('',(-0.0897283542354298,-0.104137641631234,-0.111856108510663));
#8029=CARTESIAN_POINT('',(0.0434268042445183,-0.0746532949430514,0.0110000004));
#8030=CARTESIAN_POINT('',(-0.0221398345609468,-0.0746532949430514,0.0130020004));
#8031=CARTESIAN_POINT('',(-0.0221398345609468,-0.0746532949430514,0.0130000004));
#8032=CARTESIAN_POINT('',(-0.0221398345609468,-0.0746532949430514,-0.0130000004));
#8033=CARTESIAN_POINT('',(0.,-0.0746532949430514,0.0130000004));
#8034=CARTESIAN_POINT('',(-0.0231769772486856,-0.0746532949430514,0.0130000004));
#8035=CARTESIAN_POINT('',(-0.0231769772486856,-0.0746532949430514,0.0130020004));
#8036=CARTESIAN_POINT('',(-0.0231769772486856,-0.0746532949430514,-0.0130000004));
#8037=CARTESIAN_POINT('',(0.,-0.0746532949430514,-0.0130000004));
#8038=CARTESIAN_POINT('',(-5.08934448853094E-19,-0.0684221052,0.0130020004));
#8039=CARTESIAN_POINT('',(-5.08934448853094E-19,-0.0684221052,0.0130000004));
#8040=CARTESIAN_POINT('',(0.0221398345609468,-0.0746532949430514,0.0130000004));
#8041=CARTESIAN_POINT('',(-5.08934448853094E-19,-0.0684221052,-0.0130000004));
#8042=CARTESIAN_POINT('',(0.0221398345609468,-0.0746532949430514,-0.0130000004));
#8043=CARTESIAN_POINT('',(0.0221398345609468,-0.0746532949430514,0.0130020004));
#8044=CARTESIAN_POINT('',(-1.7347234759768E-18,-0.0684221052,0.0130020004));
#8045=CARTESIAN_POINT('',(-1.7347234759768E-18,-0.0684221052,0.0130000004));
#8046=CARTESIAN_POINT('',(0.0231769772486856,-0.0746532949430514,0.0130000004));
#8047=CARTESIAN_POINT('',(0.0231769772486856,-0.0746532949430514,0.0130020004));
#8048=CARTESIAN_POINT('',(0.0231769772486856,-0.0746532949430514,-0.0130000004));
#8049=CARTESIAN_POINT('',(-1.7347234759768E-18,-0.0684221052,-0.0130000004));
#8050=CARTESIAN_POINT('',(0.,0.,-0.0130000004));
#8051=CARTESIAN_POINT('',(0.,-0.0746532949430514,-0.0130000004));
#8052=CARTESIAN_POINT('',(0.,0.,0.0130000004));
#8053=CARTESIAN_POINT('',(0.,-0.0746532949430514,0.0130000004));
#8054=CARTESIAN_POINT('',(0.0434268042445183,-0.0746532949430514,0.0110000004));
#8055=CARTESIAN_POINT('',(-0.0897283542354298,-0.104137641631234,-0.111856108510662));
#8056=CARTESIAN_POINT('',(0.,6.12323399573677E-19,0.0125));
#8057=CARTESIAN_POINT('',(0.,6.12323399573677E-19,0.0125));
#8058=CARTESIAN_POINT('',(0.01,9.62964972193618E-35,0.0125));
#8059=CARTESIAN_POINT('',(0.,6.12323399573677E-19,-0.0125));
#8060=CARTESIAN_POINT('',(0.01,9.62964972193618E-35,-0.0125));
#8061=CARTESIAN_POINT('',(0.,6.73555739531044E-19,0.0125));
#8062=CARTESIAN_POINT('',(0.,6.73555739531044E-19,0.0125));
#8063=CARTESIAN_POINT('',(0.011,-6.74075480535533E-34,0.0125));
#8064=CARTESIAN_POINT('',(0.,6.73555739531044E-19,-0.0125));
#8065=CARTESIAN_POINT('',(0.011,-6.74075480535533E-34,-0.0125));
#8066=CARTESIAN_POINT('',(0.,0.,0.0125));
#8067=CARTESIAN_POINT('',(0.,0.,-0.0125));
#8068=CARTESIAN_POINT('',(-0.0897283542354298,-0.104137641631234,-0.0434361085106635));
#8069=CARTESIAN_POINT('',(0.,0.04,-0.01475));
#8070=CARTESIAN_POINT('',(-3.5527136788005E-18,0.04,-0.01475));
#8071=CARTESIAN_POINT('',(-2.15430680055009E-18,0.016545,-0.01475));
#8072=CARTESIAN_POINT('',(0.,0.04,-0.013));
#8073=CARTESIAN_POINT('',(0.023455,0.04,-0.013));
#8074=CARTESIAN_POINT('',(0.,0.,0.03475));
#8075=CARTESIAN_POINT('',(0.,3.5527136788005E-18,0.03475));
#8076=CARTESIAN_POINT('',(0.,-0.031,0.03475));
#8077=CARTESIAN_POINT('',(-0.0306106219790423,0.00821406172744382,0.03475));
#8078=CARTESIAN_POINT('',(-0.0306106219790423,0.00821406172744363,0.03475));
#8079=CARTESIAN_POINT('',(-0.0316168242325797,0.00220395404948401,0.03475));
#8080=CARTESIAN_POINT('',(9.14113229555369E-15,3.31512595153072E-16,0.03475));
#8081=CARTESIAN_POINT('',(0.0316168242325797,0.00220395404948389,0.03475));
#8082=CARTESIAN_POINT('',(0.0316168242325796,0.00220395404948426,0.03475));
#8083=CARTESIAN_POINT('',(0.0306106219790423,0.00821406172744343,0.03475));
#8084=CARTESIAN_POINT('',(-3.5527136788005E-18,-2.41584530158434E-16,0.03475));
#8085=CARTESIAN_POINT('',(0.,0.04,-0.01475));
#8086=CARTESIAN_POINT('',(0.,0.04,0.013));
#8087=CARTESIAN_POINT('',(0.023455,0.04,0.013));
#8088=CARTESIAN_POINT('',(0.,0.04,0.01475));
#8089=CARTESIAN_POINT('',(-2.15430680055009E-18,0.016545,0.01475));
#8090=CARTESIAN_POINT('',(0.,0.,0.01475));
#8091=CARTESIAN_POINT('',(-0.0246568360053671,0.0437763899447745,0.01475));
#8092=CARTESIAN_POINT('',(-0.0246568360053672,0.0437763899447745,0.01475));
#8093=CARTESIAN_POINT('',(-0.0292158701188273,0.016545,0.01475));
#8094=CARTESIAN_POINT('',(0.,0.0396483833793207,0.01475));
#8095=CARTESIAN_POINT('',(0.0246568360053672,0.0437763899447744,0.01475));
#8096=CARTESIAN_POINT('',(0.0292158701188273,0.016545,0.01475));
#8097=CARTESIAN_POINT('',(0.0292158701188273,0.016545,0.01475));
#8098=CARTESIAN_POINT('',(0.,0.016545,0.01475));
#8099=CARTESIAN_POINT('',(-0.0292158701188273,0.016545,0.01475));
#8100=CARTESIAN_POINT('',(-0.0246568360053672,0.0437763899447744,0.01475));
#8101=CARTESIAN_POINT('',(-0.0378009992483934,-0.0347345020250511,0.03475));
#8102=CARTESIAN_POINT('',(-0.0378009992483934,-0.0347345020250511,0.023703850251217));
#8103=CARTESIAN_POINT('',(-0.0378009992483934,-0.0347345020250511,0.01475));
#8104=CARTESIAN_POINT('',(-0.0378009992483934,-0.0347345020250514,0.0237038502512178));
#8105=CARTESIAN_POINT('',(-0.0368117095543267,-0.028825414100497,0.0263618831657078));
#8106=CARTESIAN_POINT('',(-0.0353140091295469,-0.0198795577474549,0.0300968033298601));
#8107=CARTESIAN_POINT('',(-0.0332464653126233,-0.00752999191720053,0.0336219976537701));
#8108=CARTESIAN_POINT('',(-0.0321651420015115,-0.00107118156210252,0.0345704738450062));
#8109=CARTESIAN_POINT('',(-0.0316168242325796,0.00220395404948438,0.03475));
#8110=CARTESIAN_POINT('',(-0.0306106219790424,0.00821406172744319,0.03475));
#8111=CARTESIAN_POINT('',(-0.0295634232344042,0.0144690439572817,0.0344071339197969));
#8112=CARTESIAN_POINT('',(-0.0280531226089405,0.023490162080617,0.0323086955216529));
#8113=CARTESIAN_POINT('',(-0.0260933521506431,0.0351959910399979,0.0280191209876104));
#8114=CARTESIAN_POINT('',(-0.0251337005339458,0.0409280489134541,0.0255827730094403));
#8115=CARTESIAN_POINT('',(-0.0246568360053672,0.0437763899447744,0.0243187471298646));
#8116=CARTESIAN_POINT('',(-0.0246568360053672,0.0437763899447744,0.0243187471298645));
#8117=CARTESIAN_POINT('',(-0.0246568360053672,0.0437763899447744,0.01475));
#8118=CARTESIAN_POINT('',(-0.0292158701188273,0.016545,0.01475));
#8119=CARTESIAN_POINT('',(-0.0301785005652825,0.0107951493939822,0.0180696777951845));
#8120=CARTESIAN_POINT('',(-0.0328228982644232,-0.00500000000000008,9.74398446444435E-16));
#8121=CARTESIAN_POINT('',(-0.0359925369038936,-0.0239324456951552,0.01475));
#8122=CARTESIAN_POINT('',(-0.0359925369038936,-0.0239324456951552,0.01475));
#8123=CARTESIAN_POINT('',(0.,0.0396483833793206,0.01475));
#8124=CARTESIAN_POINT('',(0.0246568360053672,0.0437763899447744,0.01475));
#8125=CARTESIAN_POINT('',(0.0246568360053672,0.0437763899447744,0.0243187471298645));
#8126=CARTESIAN_POINT('',(0.0246568360053672,0.0437763899447744,0.0243187471298645));
#8127=CARTESIAN_POINT('',(0.0244261853211846,0.0451540806059303,0.0237073608419861));
#8128=CARTESIAN_POINT('',(0.0237401730081735,0.0478513323651511,0.0225495539156216));
#8129=CARTESIAN_POINT('',(0.0220160563070537,0.0517517948752077,0.0209652302526427));
#8130=CARTESIAN_POINT('',(0.0196049545771385,0.0553614641532363,0.0195673509638163));
#8131=CARTESIAN_POINT('',(0.017099633522645,0.0579907667344688,0.0185880719938733));
#8132=CARTESIAN_POINT('',(0.0147739750807182,0.0598569590563098,0.0179084194319801));
#8133=CARTESIAN_POINT('',(0.0123188659295968,0.0614896150378863,0.0173219949128185));
#8134=CARTESIAN_POINT('',(0.00963379108842836,0.0628045261969582,0.0168584228983841));
#8135=CARTESIAN_POINT('',(0.00675058877664492,0.0637552942897914,0.0165267592659007));
#8136=CARTESIAN_POINT('',(0.00455868160860307,0.0642632338451499,0.016350624923397));
#8137=CARTESIAN_POINT('',(0.00232530241794498,0.0645748845481871,0.0162429673551511));
#8138=CARTESIAN_POINT('',(-0.000730145584882101,0.0647186399709299,0.0161934340105266));
#8139=CARTESIAN_POINT('',(-0.00448154172001927,0.0643831294290258,0.0163089192735986));
#8140=CARTESIAN_POINT('',(-0.00889253724512921,0.063158749299646,0.0167337022307577));
#8141=CARTESIAN_POINT('',(-0.0129159464029183,0.0612090163507092,0.0174206501423198));
#8142=CARTESIAN_POINT('',(-0.0165490656269635,0.0585607841848676,0.018376082990071));
#8143=CARTESIAN_POINT('',(-0.019573225286212,0.0554035625895421,0.0195512513532641));
#8144=CARTESIAN_POINT('',(-0.0220017012360611,0.0517767203594562,0.0209554657275274));
#8145=CARTESIAN_POINT('',(-0.0237257985583774,0.0478972977786982,0.0225301676982113));
#8146=CARTESIAN_POINT('',(-0.02442605904778,0.0451548348447085,0.0237070261287883));
#8147=CARTESIAN_POINT('',(-0.0246568360053672,0.0437763899447744,0.0243187471298645));
#8148=CARTESIAN_POINT('',(0.0380113643198406,-0.035991025479093,0.01475));
#8149=CARTESIAN_POINT('',(0.0316168242325796,0.00220395404948427,0.03475));
#8150=CARTESIAN_POINT('',(0.0321613770800548,-0.00104869345568607,0.0345717065277884));
#8151=CARTESIAN_POINT('',(0.0332369380205949,-0.00747308481848439,0.0336336993032955));
#8152=CARTESIAN_POINT('',(0.0353058383379611,-0.0198307531089519,0.0301170420907904));
#8153=CARTESIAN_POINT('',(0.0368117177997724,-0.0288254633510492,0.0263618610117663));
#8154=CARTESIAN_POINT('',(0.0378009992483934,-0.0347345020250515,0.0237038502512177));
#8155=CARTESIAN_POINT('',(0.0378009992483934,-0.0347345020250512,0.023703850251217));
#8156=CARTESIAN_POINT('',(0.0378009992483934,-0.0347345020250512,0.03475));
#8157=CARTESIAN_POINT('',(0.0378009992483933,-0.0347345020250512,0.01475));
#8158=CARTESIAN_POINT('',(0.0378009992483934,-0.0347345020250512,0.01475));
#8159=CARTESIAN_POINT('',(0.0359925369038936,-0.0239324456951552,0.01475));
#8160=CARTESIAN_POINT('',(0.0328228982644231,-0.00499999999999992,-9.95936773122163E-16));
#8161=CARTESIAN_POINT('',(0.0301785005652825,0.0107951493939822,0.0180696777951845));
#8162=CARTESIAN_POINT('',(0.0292158701188273,0.016545,0.01475));
#8163=CARTESIAN_POINT('',(0.0246568360053672,0.0437763899447744,0.0243187471298645));
#8164=CARTESIAN_POINT('',(0.0256113237094467,0.0380751764376103,0.0268488098361206));
#8165=CARTESIAN_POINT('',(0.0275367186777366,0.0265746743851222,0.0315652051820333));
#8166=CARTESIAN_POINT('',(0.0295518358256032,0.0145382562596371,0.0344033400559715));
#8167=CARTESIAN_POINT('',(0.0306106219790424,0.00821406172744323,0.03475));
#8168=CARTESIAN_POINT('',(-0.0776088178345611,0.016545,0.01475));
#8169=CARTESIAN_POINT('',(-0.0301785005652825,0.0107951493939822,0.0180696777951845));
#8170=CARTESIAN_POINT('',(0.,0.04,-0.01175));
#8171=CARTESIAN_POINT('',(-0.00299951436620848,0.0628035723860738,-0.000162163751728459));
#8172=CARTESIAN_POINT('',(-0.00298616956258704,0.0628053277220141,-0.000995832260055065));
#8173=CARTESIAN_POINT('',(-0.00254014574668273,0.0628722334227876,-0.00223100782570009));
#8174=CARTESIAN_POINT('',(-0.00117231465122705,0.0629802629940287,-0.0032232282026831));
#8175=CARTESIAN_POINT('',(8.01521282900886E-5,0.0630117090883974,-0.00346781061358092));
#8176=CARTESIAN_POINT('',(0.00131266368591674,0.0629721307884194,-0.00315684322603784));
#8177=CARTESIAN_POINT('',(0.00263020704257935,0.0628607368680939,-0.00209512290266155));
#8178=CARTESIAN_POINT('',(0.00302049641875689,0.0628008132477051,-0.000835904596421582));
#8179=CARTESIAN_POINT('',(0.00299869834880741,0.0628036797077327,-1.91430325382278E-6));
#8180=CARTESIAN_POINT('',(-0.00301347071341734,0.0627996817593204,-0.000162387542955616));
#8181=CARTESIAN_POINT('',(0.00299869834880741,0.0628036797077327,-1.91430325382258E-6));
#8182=CARTESIAN_POINT('',(0.00299869834880741,0.0628036797077327,-1.91430325382263E-6));
#8183=CARTESIAN_POINT('',(0.00302130816342431,0.0628007065027663,0.000854614323236115));
#8184=CARTESIAN_POINT('',(0.00259825946404886,0.0628658285166061,0.00214294347958513));
#8185=CARTESIAN_POINT('',(0.00120652330326989,0.0629790253939967,0.00318205761014775));
#8186=CARTESIAN_POINT('',(-8.18799057279445E-5,0.0630123973788089,0.00343928974013122));
#8187=CARTESIAN_POINT('',(-0.00134744482602329,0.0629705900264957,0.0031137978980331));
#8188=CARTESIAN_POINT('',(-0.0026872335470843,0.0628541682503654,0.00200214986129947));
#8189=CARTESIAN_POINT('',(-0.00304999645721831,0.0627969525635701,0.000694293045094904));
#8190=CARTESIAN_POINT('',(-0.0029911325100996,0.062804673343572,-0.000160791461252475));
#8191=CARTESIAN_POINT('',(0.,0.04,-0.013));
#8192=CARTESIAN_POINT('',(0.023,0.04,-0.013));
#8193=CARTESIAN_POINT('',(0.,0.04,0.013));
#8194=CARTESIAN_POINT('',(0.023,0.04,0.013));
#8195=CARTESIAN_POINT('',(-0.0776088178345611,-0.005,0.));
#8196=CARTESIAN_POINT('',(-0.0359925369038936,-0.0239324456951552,0.01475));
#8197=CARTESIAN_POINT('',(0.,0.,0.01475));
#8198=CARTESIAN_POINT('',(0.0328696320473201,-0.0355601033381419,0.01475));
#8199=CARTESIAN_POINT('',(0.0375652937683657,-0.0372778812636918,0.01475));
#8200=CARTESIAN_POINT('',(0.,-0.0235356578592935,0.01475));
#8201=CARTESIAN_POINT('',(-0.0375652937683657,-0.0372778812636917,0.01475));
#8202=CARTESIAN_POINT('',(-0.0328696320473199,-0.0355601033381419,0.01475));
#8203=CARTESIAN_POINT('',(-0.0328696320473199,-0.0355601033381419,0.6722362));
#8204=CARTESIAN_POINT('',(-0.0378009992483934,-0.0347345020250511,0.023703850251217));
#8205=CARTESIAN_POINT('',(-0.0379395336899237,-0.0355619767278518,0.0233316346023665));
#8206=CARTESIAN_POINT('',(-0.037872659461892,-0.0364376764269736,0.0230218844628341));
#8207=CARTESIAN_POINT('',(-0.0375652937683657,-0.0372778812636916,0.0228117569919867));
#8208=CARTESIAN_POINT('',(-0.0375652937683657,-0.0372778812636917,0.0228117569919868));
#8209=CARTESIAN_POINT('',(-0.0375652937683657,-0.0372778812636917,0.03475));
#8210=CARTESIAN_POINT('',(0.,0.,0.052010716339737));
#8211=CARTESIAN_POINT('',(-0.0375652937683657,-0.0372778812636917,0.0228117569919867));
#8212=CARTESIAN_POINT('',(-0.0368723820726594,-0.039172002079426,0.0223380548671046));
#8213=CARTESIAN_POINT('',(-0.0352157180117104,-0.0428159221045996,0.0214491533403092));
#8214=CARTESIAN_POINT('',(-0.0319460092255036,-0.0478638720648067,0.0202662014447962));
#8215=CARTESIAN_POINT('',(-0.0278553048475434,-0.0524566122744212,0.0192266496656653));
#8216=CARTESIAN_POINT('',(-0.0231991299966274,-0.0563114964548188,0.018378556689204));
#8217=CARTESIAN_POINT('',(-0.0178753310411592,-0.0594966216850981,0.017693286407371));
#8218=CARTESIAN_POINT('',(-0.0131542346956908,-0.0614064131407065,0.0172893487407261));
#8219=CARTESIAN_POINT('',(-0.00921290916609484,-0.0625013441622402,0.017059391860532));
#8220=CARTESIAN_POINT('',(-0.00514084969644836,-0.0632982746320762,0.0168927558921429));
#8221=CARTESIAN_POINT('',(-0.00105859844217804,-0.0636123136064291,0.0168274299026073));
#8222=CARTESIAN_POINT('',(0.00302765394536762,-0.0634608055949469,0.0168589666787993));
#8223=CARTESIAN_POINT('',(0.00714179578061486,-0.0629880118531215,0.0169575656489395));
#8224=CARTESIAN_POINT('',(0.012138786389917,-0.0618126013351542,0.0172034657543907));
#8225=CARTESIAN_POINT('',(0.0168785934868732,-0.0599024129561901,0.0176074426371329));
#8226=CARTESIAN_POINT('',(0.0205024280655964,-0.0579276333929854,0.018030809406638));
#8227=CARTESIAN_POINT('',(0.0239104204872156,-0.0557140964769394,0.0185100961237082));
#8228=CARTESIAN_POINT('',(0.0278285765558024,-0.052485794077695,0.0192200913642277));
#8229=CARTESIAN_POINT('',(0.0319146778455702,-0.0479016398645519,0.0202576003571143));
#8230=CARTESIAN_POINT('',(0.0351896104969302,-0.042869047811016,0.021436316620234));
#8231=CARTESIAN_POINT('',(0.036872298394842,-0.039172230818379,0.0223379976616047));
#8232=CARTESIAN_POINT('',(0.0375652937683656,-0.0372778812636917,0.0228117569919867));
#8233=CARTESIAN_POINT('',(0.0375652937683657,-0.0372778812636918,0.0228117569919868));
#8234=CARTESIAN_POINT('',(0.0375652937683657,-0.0372778812636917,0.0228117569919867));
#8235=CARTESIAN_POINT('',(0.0378729252083338,-0.0364369499911663,0.0230220661377213));
#8236=CARTESIAN_POINT('',(0.0379396433028291,-0.0355626314524483,0.0233313400933747));
#8237=CARTESIAN_POINT('',(0.0378009992483934,-0.0347345020250512,0.023703850251217));
#8238=CARTESIAN_POINT('',(0.,0.,0.052010716339737));
#8239=CARTESIAN_POINT('',(0.0328696320473199,-0.0355601033381419,0.6722362));
#8240=CARTESIAN_POINT('',(0.0375652937683657,-0.0372778812636918,0.03475));
#8241=CARTESIAN_POINT('',(0.,-0.042724949124795,-0.0545862509068234));
#8242=CARTESIAN_POINT('',(-9.60170206471803E-16,0.0629999999999978,-6.68354260824344E-17));
#8243=CARTESIAN_POINT('',(8.09786277180737E-17,-0.0290000000000004,-0.0475));
#8244=CARTESIAN_POINT('',(-0.0029997619807752,-0.028844434958215,-0.0474622103361266));
#8245=CARTESIAN_POINT('',(0.0029997619807752,-0.028844434958215,-0.0474622103361266));
#8246=CARTESIAN_POINT('',(-0.0029997619807752,-0.028844434958215,-0.0474622103361266));
#8247=CARTESIAN_POINT('',(-0.00300915492826778,-0.0288434581109716,-0.0466225739694568));
#8248=CARTESIAN_POINT('',(-0.00259693992861547,-0.0288930415527731,-0.0453675967135918));
#8249=CARTESIAN_POINT('',(-0.00125704785411636,-0.0289806255271393,-0.0443171156875614));
#8250=CARTESIAN_POINT('',(-4.87566413189158E-6,-0.0290095691748998,-0.0440282561890832));
#8251=CARTESIAN_POINT('',(0.00124683950271356,-0.0289810952366406,-0.0443123258170411));
#8252=CARTESIAN_POINT('',(0.00259350062251134,-0.0288934852584709,-0.0453594477105172));
#8253=CARTESIAN_POINT('',(0.0030091625757541,-0.0288434573156488,-0.0466218903600113));
#8254=CARTESIAN_POINT('',(0.0029997619807752,-0.028844434958215,-0.0474622103361266));
#8255=CARTESIAN_POINT('',(0.,-0.029,0.04525));
#8256=CARTESIAN_POINT('',(1.57973819895899E-16,-0.0289999999999994,0.04525));
#8257=CARTESIAN_POINT('',(-0.00299978173590996,-0.0288444329037148,0.0452138124758919));
#8258=CARTESIAN_POINT('',(0.00299978173590995,-0.0288444329037148,0.0452138124758922));
#8259=CARTESIAN_POINT('',(0.00299978173590995,-0.0288444329037148,0.0452138124758922));
#8260=CARTESIAN_POINT('',(0.00300881962437,-0.0288434929756245,0.0443784326540771));
#8261=CARTESIAN_POINT('',(0.00259047495675581,-0.0288936910635023,0.0431307616648426));
#8262=CARTESIAN_POINT('',(0.00125009688665756,-0.0289808842450609,0.0420961922125352));
#8263=CARTESIAN_POINT('',(4.15924442233007E-6,-0.0290094521029003,0.0418131179333976));
#8264=CARTESIAN_POINT('',(-0.00124075947786621,-0.0289813054046344,0.0420919385455001));
#8265=CARTESIAN_POINT('',(-0.00258736867356594,-0.0288940972630226,0.0431234114486747));
#8266=CARTESIAN_POINT('',(-0.00300882587110642,-0.0288434923259724,0.0443778552628386));
#8267=CARTESIAN_POINT('',(-0.00299978173590996,-0.0288444329037148,0.0452138124758919));
#8268=CARTESIAN_POINT('',(0.,-0.0235356578592935,0.01475));
#8269=CARTESIAN_POINT('',(0.,0.,0.040025));
#8270=CARTESIAN_POINT('',(-1.77635683940025E-18,-1.77635683940025E-18,0.03525));
#8271=CARTESIAN_POINT('',(-3.85185988877447E-34,0.031,0.03525));
#8272=CARTESIAN_POINT('',(0.,0.,-0.03475));
#8273=CARTESIAN_POINT('',(0.,0.,-0.0582267070030276));
#8274=CARTESIAN_POINT('',(0.,-0.029,-0.0582267070030276));
#8275=CARTESIAN_POINT('',(0.,-1.77635683940025E-18,-0.03525));
#8276=CARTESIAN_POINT('',(-0.029,-7.10295143505464E-18,-0.03525));
#8277=CARTESIAN_POINT('',(-3.04987242545569E-5,-0.0291479853908251,-0.0474999612573823));
#8278=CARTESIAN_POINT('',(-0.00293657158878645,-0.0288509366798365,-0.0481136345035384));
#8279=CARTESIAN_POINT('',(3.05022327937685E-5,-0.0291479966421305,-0.047499961485425));
#8280=CARTESIAN_POINT('',(0.00293657158878639,-0.0288509366798365,-0.0481136345035382));
#8281=CARTESIAN_POINT('',(0.00293657158878639,-0.0288509366798365,-0.0481136345035382));
#8282=CARTESIAN_POINT('',(0.00280389719458576,-0.0288644408464738,-0.0488351566656889));
#8283=CARTESIAN_POINT('',(0.00230583590197879,-0.0289167653919492,-0.0498467610228945));
#8284=CARTESIAN_POINT('',(0.00109971947815042,-0.0289851551437462,-0.0507117731397796));
#8285=CARTESIAN_POINT('',(1.04397156723601E-5,-0.0290072736075878,-0.0509568367298539));
#8286=CARTESIAN_POINT('',(-0.00108651055265419,-0.0289857417435524,-0.0507183410275081));
#8287=CARTESIAN_POINT('',(-0.00229752899548612,-0.0289175088319034,-0.0498589259558951));
#8288=CARTESIAN_POINT('',(-0.0028037279324821,-0.0288644580746938,-0.0488360771625165));
#8289=CARTESIAN_POINT('',(-0.00293657158878634,-0.0288509366798365,-0.0481136345035385));
#8290=CARTESIAN_POINT('',(3.04866257696342E-5,0.029147946587811,-0.0475000395289292));
#8291=CARTESIAN_POINT('',(0.00299976198077498,0.0288444349582151,-0.0475377896638955));
#8292=CARTESIAN_POINT('',(0.00293657158878635,0.0288509366798365,-0.0468863654964615));
#8293=CARTESIAN_POINT('',(0.00293657158878637,0.0288509366798365,-0.0468863654964617));
#8294=CARTESIAN_POINT('',(0.00280389719458545,0.0288644408464739,-0.0461648433343095));
#8295=CARTESIAN_POINT('',(0.00230583590197662,0.0289167653919494,-0.0451532389771017));
#8296=CARTESIAN_POINT('',(0.00109971947814396,0.0289851551437465,-0.044288226860217));
#8297=CARTESIAN_POINT('',(1.04397156625072E-5,0.0290072736075879,-0.0440431632701459));
#8298=CARTESIAN_POINT('',(-0.00108651055266498,0.028985741743552,-0.0442816589724958));
#8299=CARTESIAN_POINT('',(-0.00229752899549738,0.0289175088319024,-0.0451410740441204));
#8300=CARTESIAN_POINT('',(-0.00280372793248197,0.0288644580746939,-0.0461639228374824));
#8301=CARTESIAN_POINT('',(-0.00293657158878641,0.0288509366798365,-0.0468863654964619));
#8302=CARTESIAN_POINT('',(-0.00293657158879015,0.0288509366798361,-0.0468863654964798));
#8303=CARTESIAN_POINT('',(-3.0487773813507E-5,0.0291479502701906,-0.0475000394543178));
#8304=CARTESIAN_POINT('',(-0.00299976198077519,0.028844434958215,-0.0475377896638737));
#8305=CARTESIAN_POINT('',(-0.00299976198077519,0.028844434958215,-0.0475377896638734));
#8306=CARTESIAN_POINT('',(-0.00300915492826783,0.0288434581109716,-0.0483774260305414));
#8307=CARTESIAN_POINT('',(-0.00259693992861748,0.0288930415527728,-0.0496324032864039));
#8308=CARTESIAN_POINT('',(-0.00125704785412371,0.028980625527139,-0.0506828843124349));
#8309=CARTESIAN_POINT('',(-4.8756641433718E-6,0.0290095691748998,-0.050971743810917));
#8310=CARTESIAN_POINT('',(0.00124683950270104,0.0289810952366412,-0.050687674182964));
#8311=CARTESIAN_POINT('',(0.00259350062249991,0.028893485258472,-0.0496405522895028));
#8312=CARTESIAN_POINT('',(0.00300916257575402,0.0288434573156488,-0.0483781096399874));
#8313=CARTESIAN_POINT('',(0.0029997619807752,0.028844434958215,-0.047537789663874));
#8314=CARTESIAN_POINT('',(0.,-0.029,-0.0475));
#8315=CARTESIAN_POINT('',(0.,0.029,-0.0475));
#8316=CARTESIAN_POINT('',(5.25708289276628E-16,0.0290000000000022,-0.0475));
#8317=CARTESIAN_POINT('',(0.,-0.029,-0.0475));
#8318=CARTESIAN_POINT('',(0.,0.,0.03475));
#8319=CARTESIAN_POINT('',(0.,0.,0.05475));
#8320=CARTESIAN_POINT('',(-0.029,0.,0.05475));
#8321=CARTESIAN_POINT('',(0.,-1.77635683940025E-18,0.03525));
#8322=CARTESIAN_POINT('',(0.029,-7.10295143505464E-18,0.03525));
#8323=CARTESIAN_POINT('',(0.00293126735069296,-0.028851476075216,0.0458884917530881));
#8324=CARTESIAN_POINT('',(0.00297968219936272,-0.0288465571981081,0.0456662228443543));
#8325=CARTESIAN_POINT('',(0.00300252637978852,-0.0288441474644896,0.0454413310138827));
#8326=CARTESIAN_POINT('',(0.00299978173590996,-0.0288444329037148,0.0452138124758922));
#8327=CARTESIAN_POINT('',(0.00293126735069295,-0.028851476075216,0.0458884917530881));
#8328=CARTESIAN_POINT('',(-3.03426997834468E-5,-0.0291474821613309,0.0452499544771244));
#8329=CARTESIAN_POINT('',(-0.00293126735069299,-0.028851476075216,0.045888491753088));
#8330=CARTESIAN_POINT('',(-0.00293126735069298,-0.028851476075216,0.045888491753088));
#8331=CARTESIAN_POINT('',(-0.00279340273508677,-0.0288654829165121,0.0466007213942467));
#8332=CARTESIAN_POINT('',(-0.00228610200596045,-0.0289182971695779,0.0475964784080196));
#8333=CARTESIAN_POINT('',(-0.0010888098504506,-0.028985444454822,0.0484335917950664));
#8334=CARTESIAN_POINT('',(-1.20064574058231E-5,-0.029007083304106,0.0486708430585802));
#8335=CARTESIAN_POINT('',(0.00107164560000882,-0.0289862101168382,0.0484423158488964));
#8336=CARTESIAN_POINT('',(0.00228223772074259,-0.0289187855098398,0.0476048968650648));
#8337=CARTESIAN_POINT('',(0.00279317831835183,-0.0288655057169208,0.0466018807653434));
#8338=CARTESIAN_POINT('',(0.00293126735069296,-0.028851476075216,0.0458884917530881));
#8339=CARTESIAN_POINT('',(-0.00235329472491155,0.0289222292213958,0.0429007124101602));
#8340=CARTESIAN_POINT('',(5.94732789712727E-7,0.0290388471998873,0.0419247819883626));
#8341=CARTESIAN_POINT('',(0.00235091579375268,0.0289223819790551,0.0429001596363893));
#8342=CARTESIAN_POINT('',(0.00332394666285095,0.0288054625306398,0.0452469399202865));
#8343=CARTESIAN_POINT('',(0.00235329301180312,0.0289222295931621,0.0475992920377153));
#8344=CARTESIAN_POINT('',(-6.06452073458359E-7,0.0290388471987158,0.0485752179920553));
#8345=CARTESIAN_POINT('',(-0.00235091745396515,0.0289223816119677,0.0475998359939933));
#8346=CARTESIAN_POINT('',(-0.00332394581952071,0.0288054627153532,0.0452530600601599));
#8347=CARTESIAN_POINT('',(-0.00235329472491155,0.0289222292213958,0.0429007124101602));
#8348=CARTESIAN_POINT('',(5.94732789712727E-7,0.0290388471998873,0.0419247819883626));
#8349=CARTESIAN_POINT('',(0.00235091579375268,0.0289223819790551,0.0429001596363893));
#8350=CARTESIAN_POINT('',(-2.98657244279343E-18,0.029,0.04225));
#8351=CARTESIAN_POINT('',(0.,-0.029,0.04525));
#8352=CARTESIAN_POINT('',(0.,-0.029,0.04525));
#8353=CARTESIAN_POINT('',(0.,0.,0.03525));
#8354=CARTESIAN_POINT('',(0.,0.,-0.01475));
#8355=CARTESIAN_POINT('',(0.0292158701188273,0.016545,-0.01475));
#8356=CARTESIAN_POINT('',(0.0292158701188273,0.016545,-0.01475));
#8357=CARTESIAN_POINT('',(0.0246568360053672,0.0437763899447744,-0.01475));
#8358=CARTESIAN_POINT('',(-1.77635683940025E-18,0.0396483833793206,-0.01475));
#8359=CARTESIAN_POINT('',(-0.0246568360053672,0.0437763899447744,-0.01475));
#8360=CARTESIAN_POINT('',(-0.0246568360053672,0.0437763899447744,-0.01475));
#8361=CARTESIAN_POINT('',(-0.0292158701188273,0.016545,-0.01475));
#8362=CARTESIAN_POINT('',(0.,0.016545,-0.01475));
#8363=CARTESIAN_POINT('',(0.0292158701188272,0.016545,-0.01475));
#8364=CARTESIAN_POINT('',(0.,0.,-0.03525));
#8365=CARTESIAN_POINT('',(0.,-1.77635683940025E-18,-0.03525));
#8366=CARTESIAN_POINT('',(3.79640507735679E-18,0.031,-0.03525));
#8367=CARTESIAN_POINT('',(0.,-0.029,-0.0475));
#8368=CARTESIAN_POINT('',(0.,0.029,-0.0475));
#8369=CARTESIAN_POINT('',(0.,-0.0791723446654833,-0.103349851865331));
#8370=CARTESIAN_POINT('',(0.,0.00822406222571555,-0.0582267070030276));
#8371=CARTESIAN_POINT('',(0.,0.00168477969117994,-0.0582267070030276));
#8372=CARTESIAN_POINT('',(0.,-0.047070468643187,0.054137920718524));
#8373=CARTESIAN_POINT('',(0.0246568360053672,0.0437763899447744,-0.01475));
#8374=CARTESIAN_POINT('',(0.0328228982644231,-0.005,2.50977123598683E-16));
#8375=CARTESIAN_POINT('',(0.0359925369038936,-0.0239324456951552,-0.01475));
#8376=CARTESIAN_POINT('',(0.0301785005652825,0.0107951493939822,-0.0180696777951845));
#8377=CARTESIAN_POINT('',(0.0378009992483933,-0.0347345020250512,-0.01475));
#8378=CARTESIAN_POINT('',(0.0378009992483933,-0.0347345020250512,-0.01475));
#8379=CARTESIAN_POINT('',(0.0378009992483933,-0.0347345020250512,-0.0237038502512179));
#8380=CARTESIAN_POINT('',(0.0378009992483934,-0.0347345020250516,-0.0237038502512177));
#8381=CARTESIAN_POINT('',(0.0316168242325796,0.00220395404948403,-0.03475));
#8382=CARTESIAN_POINT('',(0.0327062789897151,-0.00430342593066477,-0.0343932987682137));
#8383=CARTESIAN_POINT('',(0.034275406372161,-0.0136759198758738,-0.0321451100959277));
#8384=CARTESIAN_POINT('',(0.0363102609424209,-0.0258302308339899,-0.0276010341206553));
#8385=CARTESIAN_POINT('',(0.0373060148884253,-0.0317779301312242,-0.0250337789150296));
#8386=CARTESIAN_POINT('',(0.0378009992483935,-0.0347345020250519,-0.0237038502512176));
#8387=CARTESIAN_POINT('',(0.0316168242325797,0.0022039540494836,-0.03475));
#8388=CARTESIAN_POINT('',(0.0306106219790425,0.00821406172744211,-0.03475));
#8389=CARTESIAN_POINT('',(0.0306106219790424,0.008214061727443,-0.03475));
#8390=CARTESIAN_POINT('',(0.0246568360053671,0.0437763899447746,-0.0243187471298645));
#8391=CARTESIAN_POINT('',(0.0256113237094466,0.0380751764376104,-0.0268488098361205));
#8392=CARTESIAN_POINT('',(0.0275367186777367,0.0265746743851218,-0.0315652051820334));
#8393=CARTESIAN_POINT('',(0.0295518358256032,0.0145382562596374,-0.0344033400559715));
#8394=CARTESIAN_POINT('',(0.0306106219790423,0.00821406172744344,-0.03475));
#8395=CARTESIAN_POINT('',(0.0246568360053672,0.0437763899447745,-0.0243187471298645));
#8396=CARTESIAN_POINT('',(0.0246568360053672,0.0437763899447744,-0.01475));
#8397=CARTESIAN_POINT('',(0.0301785005652825,0.0107951493939822,-0.0180696777951845));
#8398=CARTESIAN_POINT('',(0.,0.0396483833793206,-0.01475));
#8399=CARTESIAN_POINT('',(-0.0246568360053672,0.0437763899447744,-0.01475));
#8400=CARTESIAN_POINT('',(-0.0246568360053672,0.0437763899447744,-0.0243187471298645));
#8401=CARTESIAN_POINT('',(0.0246568360053672,0.0437763899447746,-0.0243187471298645));
#8402=CARTESIAN_POINT('',(0.0244261853211846,0.0451540806059305,-0.023707360841986));
#8403=CARTESIAN_POINT('',(0.0237401730081734,0.0478513323651514,-0.0225495539156214));
#8404=CARTESIAN_POINT('',(0.0220160563070535,0.0517517948752079,-0.0209652302526425));
#8405=CARTESIAN_POINT('',(0.0196049545771384,0.0553614641532365,-0.0195673509638162));
#8406=CARTESIAN_POINT('',(0.0170996335226448,0.057990766734469,-0.0185880719938732));
#8407=CARTESIAN_POINT('',(0.014773975080718,0.0598569590563099,-0.01790841943198));
#8408=CARTESIAN_POINT('',(0.0123188659295966,0.0614896150378864,-0.0173219949128184));
#8409=CARTESIAN_POINT('',(0.00963379108842817,0.0628045261969582,-0.016858422898384));
#8410=CARTESIAN_POINT('',(0.00675058877664476,0.0637552942897915,-0.0165267592659006));
#8411=CARTESIAN_POINT('',(0.00455868160860291,0.0642632338451499,-0.016350624923397));
#8412=CARTESIAN_POINT('',(0.00232530241794481,0.0645748845481871,-0.0162429673551511));
#8413=CARTESIAN_POINT('',(-0.000730145584882256,0.0647186399709299,-0.0161934340105266));
#8414=CARTESIAN_POINT('',(-0.00448154172001943,0.0643831294290258,-0.0163089192735985));
#8415=CARTESIAN_POINT('',(-0.00889253724512927,0.063158749299646,-0.0167337022307577));
#8416=CARTESIAN_POINT('',(-0.0129159464029183,0.0612090163507091,-0.0174206501423198));
#8417=CARTESIAN_POINT('',(-0.0165490656269636,0.0585607841848676,-0.018376082990071));
#8418=CARTESIAN_POINT('',(-0.019573225286212,0.0554035625895421,-0.0195512513532641));
#8419=CARTESIAN_POINT('',(-0.0220017012360611,0.0517767203594562,-0.0209554657275274));
#8420=CARTESIAN_POINT('',(-0.0237257985583774,0.0478972977786982,-0.0225301676982113));
#8421=CARTESIAN_POINT('',(-0.02442605904778,0.0451548348447085,-0.0237070261287883));
#8422=CARTESIAN_POINT('',(-0.0246568360053672,0.0437763899447745,-0.0243187471298645));
#8423=CARTESIAN_POINT('',(-0.0380113643198406,-0.035991025479093,-0.01475));
#8424=CARTESIAN_POINT('',(-0.0306106219790426,0.00821406172744194,-0.03475));
#8425=CARTESIAN_POINT('',(-0.0295634232344044,0.0144690439572807,-0.0344071339197971));
#8426=CARTESIAN_POINT('',(-0.0280531226089406,0.0234901620806161,-0.0323086955216532));
#8427=CARTESIAN_POINT('',(-0.0260933521506431,0.0351959910399975,-0.0280191209876106));
#8428=CARTESIAN_POINT('',(-0.0251337005339458,0.0409280489134541,-0.0255827730094403));
#8429=CARTESIAN_POINT('',(-0.0246568360053671,0.0437763899447745,-0.0243187471298645));
#8430=CARTESIAN_POINT('',(-0.0306106219790425,0.00821406172744216,-0.03475));
#8431=CARTESIAN_POINT('',(-0.0316168242325796,0.00220395404948424,-0.03475));
#8432=CARTESIAN_POINT('',(-0.0316168242325796,0.00220395404948406,-0.03475));
#8433=CARTESIAN_POINT('',(-0.0378009992482983,-0.0347345020242971,-0.0237038502515795));
#8434=CARTESIAN_POINT('',(-0.0368102789739022,-0.02881686915583,-0.0263657268628202));
#8435=CARTESIAN_POINT('',(-0.0348121591335525,-0.0168819769893,-0.03134699023701));
#8436=CARTESIAN_POINT('',(-0.0327195944738099,-0.00438296013257355,-0.0343889391107361));
#8437=CARTESIAN_POINT('',(-0.0316168242325796,0.00220395404948413,-0.03475));
#8438=CARTESIAN_POINT('',(-0.0378009992483299,-0.0347345020246722,-0.0237038502513883));
#8439=CARTESIAN_POINT('',(-0.0378009992483934,-0.0347345020250511,-0.0237038502512179));
#8440=CARTESIAN_POINT('',(-0.0378009992483934,-0.0347345020250511,-0.01475));
#8441=CARTESIAN_POINT('',(-0.0359925369038936,-0.0239324456951552,-0.01475));
#8442=CARTESIAN_POINT('',(-0.0359925369038936,-0.0239324456951552,-0.01475));
#8443=CARTESIAN_POINT('',(-0.0328228982644232,-0.00500000000000008,-2.87703087949443E-16));
#8444=CARTESIAN_POINT('',(-0.0301785005652825,0.0107951493939822,-0.0180696777951845));
#8445=CARTESIAN_POINT('',(-0.0301785005652825,0.0107951493939822,-0.0180696777951845));
#8446=CARTESIAN_POINT('',(-0.0776088178345611,0.0078847459621556,-0.01975));
#8447=CARTESIAN_POINT('',(-0.0301785005652825,0.0107951493939822,-0.0180696777951845));
#8448=CARTESIAN_POINT('',(0.,0.,0.040025));
#8449=CARTESIAN_POINT('',(0.,3.5527136788005E-18,-0.03475));
#8450=CARTESIAN_POINT('',(0.,-0.031,-0.03475));
#8451=CARTESIAN_POINT('',(-0.0776088178345611,-0.005,0.));
#8452=CARTESIAN_POINT('',(-0.0359925369038936,-0.0239324456951552,-0.01475));
#8453=CARTESIAN_POINT('',(0.,0.,-0.01475));
#8454=CARTESIAN_POINT('',(-0.03286963204732,-0.0355601033381419,-0.01475));
#8455=CARTESIAN_POINT('',(-0.0375652937683657,-0.0372778812636917,-0.01475));
#8456=CARTESIAN_POINT('',(3.5527136788005E-18,-0.0235356578592935,-0.01475));
#8457=CARTESIAN_POINT('',(0.0375652937683657,-0.0372778812636918,-0.01475));
#8458=CARTESIAN_POINT('',(0.0328696320473203,-0.035560103338142,-0.01475));
#8459=CARTESIAN_POINT('',(0.0328696320473199,-0.0355601033381419,-0.77707293494511));
#8460=CARTESIAN_POINT('',(0.0375652937683657,-0.0372778812636918,-0.0228117569919877));
#8461=CARTESIAN_POINT('',(0.0375652937683657,-0.0372778812636918,-0.0228117569919877));
#8462=CARTESIAN_POINT('',(0.0378009992483935,-0.0347345020250519,-0.0237038502512175));
#8463=CARTESIAN_POINT('',(0.0379395343785947,-0.0355619808413266,-0.0233316327520394));
#8464=CARTESIAN_POINT('',(0.0378726603922854,-0.0364376738836806,-0.0230218850988891));
#8465=CARTESIAN_POINT('',(0.0375652937683657,-0.0372778812636918,-0.0228117569919877));
#8466=CARTESIAN_POINT('',(0.,0.,-0.052010716339737));
#8467=CARTESIAN_POINT('',(1.77635683940025E-18,5.32907051820075E-18,-0.03475));
#8468=CARTESIAN_POINT('',(-0.0375652937683657,-0.0372778812636917,-0.0228117569919877));
#8469=CARTESIAN_POINT('',(-0.0368723814300125,-0.0391720038361446,-0.0223380544277665));
#8470=CARTESIAN_POINT('',(-0.0352157157828944,-0.0428159259480469,-0.0214491524280103));
#8471=CARTESIAN_POINT('',(-0.0319460093286459,-0.0478638717967643,-0.0202662015107985));
#8472=CARTESIAN_POINT('',(-0.0278553031209884,-0.052456614149853,-0.0192266492426356));
#8473=CARTESIAN_POINT('',(-0.0231991281117714,-0.0563114975962444,-0.0183785564441856));
#8474=CARTESIAN_POINT('',(-0.0178753309559553,-0.0594966218536073,-0.0176932863706357));
#8475=CARTESIAN_POINT('',(-0.013154231246997,-0.0614064142875746,-0.0172893484991303));
#8476=CARTESIAN_POINT('',(-0.00921290864977878,-0.0625013442143116,-0.0170593918498272));
#8477=CARTESIAN_POINT('',(-0.0051408499180295,-0.0632982746670183,-0.0168927558847434));
#8478=CARTESIAN_POINT('',(-0.00105859515404703,-0.0636123137459811,-0.0168274298734829));
#8479=CARTESIAN_POINT('',(0.00302765575771894,-0.0634608053488871,-0.0168589667301854));
#8480=CARTESIAN_POINT('',(0.00714179333735995,-0.0629880122993201,-0.01695756555541));
#8481=CARTESIAN_POINT('',(0.0121387916213171,-0.0618125997379239,-0.0172034660910362));
#8482=CARTESIAN_POINT('',(0.0168785920660817,-0.0599024135514785,-0.0176074425106158));
#8483=CARTESIAN_POINT('',(0.0205024292275728,-0.0579276328140605,-0.0180308095300653));
#8484=CARTESIAN_POINT('',(0.0239104231105815,-0.0557140944842808,-0.0185100965594511));
#8485=CARTESIAN_POINT('',(0.0278285759269693,-0.0524857946247409,-0.0192200912425152));
#8486=CARTESIAN_POINT('',(0.031914679755287,-0.0479016376111136,-0.0202576008698634));
#8487=CARTESIAN_POINT('',(0.0351896110741646,-0.042869046351534,-0.0214363169788631));
#8488=CARTESIAN_POINT('',(0.0368722982470235,-0.0391722312224509,-0.022337997560551));
#8489=CARTESIAN_POINT('',(0.0375652937683657,-0.0372778812636918,-0.0228117569919877));
#8490=CARTESIAN_POINT('',(-0.0375652937683657,-0.0372778812636917,-0.0228117569919877));
#8491=CARTESIAN_POINT('',(-0.0375652937683657,-0.0372778812636917,-0.0228117569919877));
#8492=CARTESIAN_POINT('',(-0.0378729272452308,-0.0364369444231711,-0.0230220675302264));
#8493=CARTESIAN_POINT('',(-0.0379396435855259,-0.0355626331402284,-0.0233313393341246));
#8494=CARTESIAN_POINT('',(-0.0378009992482659,-0.0347345020242895,-0.0237038502515605));
#8495=CARTESIAN_POINT('',(0.,0.,-0.03475));
#8496=CARTESIAN_POINT('',(-3.5527136788005E-18,1.06581410364015E-17,-0.03475));
#8497=CARTESIAN_POINT('',(0.,0.,-0.052010716339737));
#8498=CARTESIAN_POINT('',(-0.0328696320473199,-0.0355601033381419,-0.77666486957853));
#8499=CARTESIAN_POINT('',(-0.0375652937683657,-0.0372778812636917,-0.0228117569919877));
#8500=CARTESIAN_POINT('',(0.,-0.0235356578592935,-0.01475));
#8501=CARTESIAN_POINT('',(-0.715243651719731,-0.0114123038947582,-0.0582267070030276));
#8502=CARTESIAN_POINT('',(-0.715243651719731,0.027040170002071,0.05475));
#8503=CARTESIAN_POINT('',(0.,0.04,-0.013));
#8504=CARTESIAN_POINT('',(0.,0.04,0.013));
#8505=CARTESIAN_POINT('',(-0.0897283542354298,-0.104137641631234,-0.220278213710662));
#8506=CARTESIAN_POINT('',(0.,0.,-0.0130000004));
#8507=CARTESIAN_POINT('',(0.,-0.0746532949430514,-0.0130000004));
#8508=CARTESIAN_POINT('',(0.0231769772486856,-0.0746532949430514,-0.0130000004));
#8509=CARTESIAN_POINT('',(0.0221398345609468,-0.0746532949430514,-0.0130000004));
#8510=CARTESIAN_POINT('',(-1.7347234759768E-18,-0.0684221052,-0.0130000004));
#8511=CARTESIAN_POINT('',(-0.0231769772486856,-0.0746532949430514,-0.0130000004));
#8512=CARTESIAN_POINT('',(0.,-0.0746532949430514,-0.0130000004));
#8513=CARTESIAN_POINT('',(-0.0221398345609468,-0.0746532949430514,-0.0130000004));
#8514=CARTESIAN_POINT('',(-5.08934448853094E-19,-0.0684221052,-0.0130000004));
#8515=CARTESIAN_POINT('',(-5.08934448853094E-19,-0.0684221052,0.0130020004));
#8516=CARTESIAN_POINT('',(-0.0221398345609468,-0.0746532949430514,0.0130020004));
#8517=CARTESIAN_POINT('',(-0.0221398345609468,-0.0746532949430514,0.0130000004));
#8518=CARTESIAN_POINT('',(-5.08934448853094E-19,-0.0684221052,0.0130000004));
#8519=CARTESIAN_POINT('',(0.0221398345609468,-0.0746532949430514,0.0130000004));
#8520=CARTESIAN_POINT('',(0.0221398345609468,-0.0746532949430514,0.0130020004));
#8521=CARTESIAN_POINT('',(-1.7347234759768E-18,-0.0684221052,0.0130020004));
#8522=CARTESIAN_POINT('',(-1.7347234759768E-18,-0.0684221052,0.0130000004));
#8523=CARTESIAN_POINT('',(-0.0231769772486856,-0.0746532949430514,0.0130000004));
#8524=CARTESIAN_POINT('',(0.0231769772486856,-0.0746532949430514,0.0130000004));
#8525=CARTESIAN_POINT('',(-0.0231769772486856,-0.0746532949430514,0.0130020004));
#8526=CARTESIAN_POINT('',(0.0231769772486856,-0.0746532949430514,0.0130020004));
#8527=CARTESIAN_POINT('',(0.,0.,0.0130000004));
#8528=CARTESIAN_POINT('',(0.,-0.0746532949430514,0.0130000004));
#8529=CARTESIAN_POINT('',(0.,-0.0746532949430514,0.0130000004));
#8530=CARTESIAN_POINT('',(0.0434268042445183,-0.0746532949430514,0.0110000004));
#8531=CARTESIAN_POINT('',(0.0434268042445183,-0.0746532949430514,0.0110000004));
#8532=CARTESIAN_POINT('',(-0.0897283542354298,-0.104137641631234,-0.111856108510662));
#8533=CARTESIAN_POINT('',(-0.0896503542354298,-0.104137641631234,-0.00512610829066364));
#8534=MECHANICAL_DESIGN_GEOMETRIC_PRESENTATION_REPRESENTATION('',(#4334,
#4335,#4336,#4337,#4338,#4339,#4340,#4341,#4342,#4343,#10,#11,#12,#13,#14,
#4344),#8535);
#8535=(
GEOMETRIC_REPRESENTATION_CONTEXT(3)
GLOBAL_UNCERTAINTY_ASSIGNED_CONTEXT((#8547))
GLOBAL_UNIT_ASSIGNED_CONTEXT((#8561,#8560,#8559))
REPRESENTATION_CONTEXT('MAS-680','TOP_LEVEL_ASSEMBLY_PART')
);
#8536=(
GEOMETRIC_REPRESENTATION_CONTEXT(3)
GLOBAL_UNCERTAINTY_ASSIGNED_CONTEXT((#8548))
GLOBAL_UNIT_ASSIGNED_CONTEXT((#8561,#8560,#8559))
REPRESENTATION_CONTEXT('Heavy hex bolt 3/8-16 x 1.5','COMPONENT_PART')
);
#8537=(
GEOMETRIC_REPRESENTATION_CONTEXT(3)
GLOBAL_UNCERTAINTY_ASSIGNED_CONTEXT((#8549))
GLOBAL_UNIT_ASSIGNED_CONTEXT((#8561,#8560,#8559))
REPRESENTATION_CONTEXT('Part 1','COMPONENT_PART')
);
#8538=(
GEOMETRIC_REPRESENTATION_CONTEXT(3)
GLOBAL_UNCERTAINTY_ASSIGNED_CONTEXT((#8550))
GLOBAL_UNIT_ASSIGNED_CONTEXT((#8561,#8560,#8559))
REPRESENTATION_CONTEXT('Part 1','COMPONENT_PART')
);
#8539=(
GEOMETRIC_REPRESENTATION_CONTEXT(3)
GLOBAL_UNCERTAINTY_ASSIGNED_CONTEXT((#8551))
GLOBAL_UNIT_ASSIGNED_CONTEXT((#8561,#8560,#8559))
REPRESENTATION_CONTEXT('Part 1','COMPONENT_PART')
);
#8540=(
GEOMETRIC_REPRESENTATION_CONTEXT(3)
GLOBAL_UNCERTAINTY_ASSIGNED_CONTEXT((#8552))
GLOBAL_UNIT_ASSIGNED_CONTEXT((#8561,#8560,#8559))
REPRESENTATION_CONTEXT('Part 1','COMPONENT_PART')
);
#8541=(
GEOMETRIC_REPRESENTATION_CONTEXT(3)
GLOBAL_UNCERTAINTY_ASSIGNED_CONTEXT((#8553))
GLOBAL_UNIT_ASSIGNED_CONTEXT((#8561,#8560,#8559))
REPRESENTATION_CONTEXT('Part 2','COMPONENT_PART')
);
#8542=(
GEOMETRIC_REPRESENTATION_CONTEXT(3)
GLOBAL_UNCERTAINTY_ASSIGNED_CONTEXT((#8554))
GLOBAL_UNIT_ASSIGNED_CONTEXT((#8561,#8560,#8559))
REPRESENTATION_CONTEXT('Part 1','COMPONENT_PART')
);
#8543=(
GEOMETRIC_REPRESENTATION_CONTEXT(3)
GLOBAL_UNCERTAINTY_ASSIGNED_CONTEXT((#8555))
GLOBAL_UNIT_ASSIGNED_CONTEXT((#8561,#8560,#8559))
REPRESENTATION_CONTEXT('Part 4','COMPONENT_PART')
);
#8544=(
GEOMETRIC_REPRESENTATION_CONTEXT(3)
GLOBAL_UNCERTAINTY_ASSIGNED_CONTEXT((#8556))
GLOBAL_UNIT_ASSIGNED_CONTEXT((#8561,#8560,#8559))
REPRESENTATION_CONTEXT('Part 2','COMPONENT_PART')
);
#8545=(
GEOMETRIC_REPRESENTATION_CONTEXT(3)
GLOBAL_UNCERTAINTY_ASSIGNED_CONTEXT((#8557))
GLOBAL_UNIT_ASSIGNED_CONTEXT((#8561,#8560,#8559))
REPRESENTATION_CONTEXT('CRANKSHAFT','COMPONENT_PART')
);
#8546=(
GEOMETRIC_REPRESENTATION_CONTEXT(3)
GLOBAL_UNCERTAINTY_ASSIGNED_CONTEXT((#8558))
GLOBAL_UNIT_ASSIGNED_CONTEXT((#8561,#8560,#8559))
REPRESENTATION_CONTEXT('Part 3','COMPONENT_PART')
);
#8547=UNCERTAINTY_MEASURE_WITH_UNIT(LENGTH_MEASURE(1.E-8),#8561,
'DISTANCE_ACCURACY_VALUE','Maximum Tolerance applied to model');
#8548=UNCERTAINTY_MEASURE_WITH_UNIT(LENGTH_MEASURE(2.E-5),#8561,
'DISTANCE_ACCURACY_VALUE','Maximum Tolerance applied to model');
#8549=UNCERTAINTY_MEASURE_WITH_UNIT(LENGTH_MEASURE(1.E-8),#8561,
'DISTANCE_ACCURACY_VALUE','Maximum Tolerance applied to model');
#8550=UNCERTAINTY_MEASURE_WITH_UNIT(LENGTH_MEASURE(1.E-8),#8561,
'DISTANCE_ACCURACY_VALUE','Maximum Tolerance applied to model');
#8551=UNCERTAINTY_MEASURE_WITH_UNIT(LENGTH_MEASURE(2.E-5),#8561,
'DISTANCE_ACCURACY_VALUE','Maximum Tolerance applied to model');
#8552=UNCERTAINTY_MEASURE_WITH_UNIT(LENGTH_MEASURE(1.E-8),#8561,
'DISTANCE_ACCURACY_VALUE','Maximum Tolerance applied to model');
#8553=UNCERTAINTY_MEASURE_WITH_UNIT(LENGTH_MEASURE(2.E-5),#8561,
'DISTANCE_ACCURACY_VALUE','Maximum Tolerance applied to model');
#8554=UNCERTAINTY_MEASURE_WITH_UNIT(LENGTH_MEASURE(2.E-5),#8561,
'DISTANCE_ACCURACY_VALUE','Maximum Tolerance applied to model');
#8555=UNCERTAINTY_MEASURE_WITH_UNIT(LENGTH_MEASURE(1.E-8),#8561,
'DISTANCE_ACCURACY_VALUE','Maximum Tolerance applied to model');
#8556=UNCERTAINTY_MEASURE_WITH_UNIT(LENGTH_MEASURE(1.E-8),#8561,
'DISTANCE_ACCURACY_VALUE','Maximum Tolerance applied to model');
#8557=UNCERTAINTY_MEASURE_WITH_UNIT(LENGTH_MEASURE(0.0002),#8561,
'DISTANCE_ACCURACY_VALUE','Maximum Tolerance applied to model');
#8558=UNCERTAINTY_MEASURE_WITH_UNIT(LENGTH_MEASURE(1.E-8),#8561,
'DISTANCE_ACCURACY_VALUE','Maximum Tolerance applied to model');
#8559=(
NAMED_UNIT(*)
SI_UNIT($,.STERADIAN.)
SOLID_ANGLE_UNIT()
);
#8560=(
NAMED_UNIT(*)
PLANE_ANGLE_UNIT()
SI_UNIT($,.RADIAN.)
);
#8561=(
LENGTH_UNIT()
NAMED_UNIT(*)
SI_UNIT($,.METRE.)
);
#8562=PRODUCT_DEFINITION_SHAPE('','',#8589);
#8563=PRODUCT_DEFINITION_SHAPE('','',#8590);
#8564=PRODUCT_DEFINITION_SHAPE(' ','NAUO PRDDFN',#72);
#8565=PRODUCT_DEFINITION_SHAPE('','',#8591);
#8566=PRODUCT_DEFINITION_SHAPE(' ','NAUO PRDDFN',#73);
#8567=PRODUCT_DEFINITION_SHAPE('','',#8592);
#8568=PRODUCT_DEFINITION_SHAPE(' ','NAUO PRDDFN',#74);
#8569=PRODUCT_DEFINITION_SHAPE('','',#8593);
#8570=PRODUCT_DEFINITION_SHAPE(' ','NAUO PRDDFN',#75);
#8571=PRODUCT_DEFINITION_SHAPE(' ','NAUO PRDDFN',#76);
#8572=PRODUCT_DEFINITION_SHAPE(' ','NAUO PRDDFN',#77);
#8573=PRODUCT_DEFINITION_SHAPE('','',#8594);
#8574=PRODUCT_DEFINITION_SHAPE(' ','NAUO PRDDFN',#78);
#8575=PRODUCT_DEFINITION_SHAPE('','',#8595);
#8576=PRODUCT_DEFINITION_SHAPE(' ','NAUO PRDDFN',#79);
#8577=PRODUCT_DEFINITION_SHAPE(' ','NAUO PRDDFN',#80);
#8578=PRODUCT_DEFINITION_SHAPE('','',#8596);
#8579=PRODUCT_DEFINITION_SHAPE(' ','NAUO PRDDFN',#81);
#8580=PRODUCT_DEFINITION_SHAPE('','',#8597);
#8581=PRODUCT_DEFINITION_SHAPE(' ','NAUO PRDDFN',#82);
#8582=PRODUCT_DEFINITION_SHAPE('','',#8598);
#8583=PRODUCT_DEFINITION_SHAPE(' ','NAUO PRDDFN',#83);
#8584=PRODUCT_DEFINITION_SHAPE('','',#8599);
#8585=PRODUCT_DEFINITION_SHAPE(' ','NAUO PRDDFN',#84);
#8586=PRODUCT_DEFINITION_SHAPE('','',#8600);
#8587=PRODUCT_DEFINITION_SHAPE(' ','NAUO PRDDFN',#85);
#8588=PRODUCT_DEFINITION_SHAPE(' ','NAUO PRDDFN',#86);
#8589=PRODUCT_DEFINITION('','',#8613,#8601);
#8590=PRODUCT_DEFINITION('','',#8614,#8602);
#8591=PRODUCT_DEFINITION('','',#8615,#8603);
#8592=PRODUCT_DEFINITION('','',#8616,#8604);
#8593=PRODUCT_DEFINITION('','',#8617,#8605);
#8594=PRODUCT_DEFINITION('','',#8618,#8606);
#8595=PRODUCT_DEFINITION('','',#8619,#8607);
#8596=PRODUCT_DEFINITION('','',#8620,#8608);
#8597=PRODUCT_DEFINITION('','',#8621,#8609);
#8598=PRODUCT_DEFINITION('','',#8622,#8610);
#8599=PRODUCT_DEFINITION('','',#8623,#8611);
#8600=PRODUCT_DEFINITION('','',#8624,#8612);
#8601=PRODUCT_DEFINITION_CONTEXT('',#8674,'design');
#8602=PRODUCT_DEFINITION_CONTEXT('',#8674,'design');
#8603=PRODUCT_DEFINITION_CONTEXT('',#8674,'design');
#8604=PRODUCT_DEFINITION_CONTEXT('',#8674,'design');
#8605=PRODUCT_DEFINITION_CONTEXT('',#8674,'design');
#8606=PRODUCT_DEFINITION_CONTEXT('',#8674,'design');
#8607=PRODUCT_DEFINITION_CONTEXT('',#8674,'design');
#8608=PRODUCT_DEFINITION_CONTEXT('',#8674,'design');
#8609=PRODUCT_DEFINITION_CONTEXT('',#8674,'design');
#8610=PRODUCT_DEFINITION_CONTEXT('',#8674,'design');
#8611=PRODUCT_DEFINITION_CONTEXT('',#8674,'design');
#8612=PRODUCT_DEFINITION_CONTEXT('',#8674,'design');
#8613=PRODUCT_DEFINITION_FORMATION_WITH_SPECIFIED_SOURCE('','',#8637,
 .NOT_KNOWN.);
#8614=PRODUCT_DEFINITION_FORMATION_WITH_SPECIFIED_SOURCE('','',#8638,
 .NOT_KNOWN.);
#8615=PRODUCT_DEFINITION_FORMATION_WITH_SPECIFIED_SOURCE('','',#8639,
 .NOT_KNOWN.);
#8616=PRODUCT_DEFINITION_FORMATION_WITH_SPECIFIED_SOURCE('','',#8640,
 .NOT_KNOWN.);
#8617=PRODUCT_DEFINITION_FORMATION_WITH_SPECIFIED_SOURCE('','',#8641,
 .NOT_KNOWN.);
#8618=PRODUCT_DEFINITION_FORMATION_WITH_SPECIFIED_SOURCE('','',#8642,
 .NOT_KNOWN.);
#8619=PRODUCT_DEFINITION_FORMATION_WITH_SPECIFIED_SOURCE('','',#8643,
 .NOT_KNOWN.);
#8620=PRODUCT_DEFINITION_FORMATION_WITH_SPECIFIED_SOURCE('','',#8644,
 .NOT_KNOWN.);
#8621=PRODUCT_DEFINITION_FORMATION_WITH_SPECIFIED_SOURCE('','',#8645,
 .NOT_KNOWN.);
#8622=PRODUCT_DEFINITION_FORMATION_WITH_SPECIFIED_SOURCE('','',#8646,
 .NOT_KNOWN.);
#8623=PRODUCT_DEFINITION_FORMATION_WITH_SPECIFIED_SOURCE('','',#8647,
 .NOT_KNOWN.);
#8624=PRODUCT_DEFINITION_FORMATION_WITH_SPECIFIED_SOURCE('','',#8648,
 .NOT_KNOWN.);
#8625=PRODUCT_RELATED_PRODUCT_CATEGORY('','',(#8637));
#8626=PRODUCT_RELATED_PRODUCT_CATEGORY('','',(#8638));
#8627=PRODUCT_RELATED_PRODUCT_CATEGORY('','',(#8639));
#8628=PRODUCT_RELATED_PRODUCT_CATEGORY('','',(#8640));
#8629=PRODUCT_RELATED_PRODUCT_CATEGORY('','',(#8641));
#8630=PRODUCT_RELATED_PRODUCT_CATEGORY('','',(#8642));
#8631=PRODUCT_RELATED_PRODUCT_CATEGORY('','',(#8643));
#8632=PRODUCT_RELATED_PRODUCT_CATEGORY('','',(#8644));
#8633=PRODUCT_RELATED_PRODUCT_CATEGORY('','',(#8645));
#8634=PRODUCT_RELATED_PRODUCT_CATEGORY('','',(#8646));
#8635=PRODUCT_RELATED_PRODUCT_CATEGORY('','',(#8647));
#8636=PRODUCT_RELATED_PRODUCT_CATEGORY('','',(#8648));
#8637=PRODUCT('MAS-680','MAS-680','MAS-680',(#8661));
#8638=PRODUCT('Heavy hex bolt 3/8-16 x 1.5',
'Heavy hex bolt 3/8-16 x 1.5','Heavy hex bolt 3/8-16 x 1.5',(#8662));
#8639=PRODUCT('Part 1','Part 1','Part 1',(#8663));
#8640=PRODUCT('Part 1','Part 1','Part 1',(#8664));
#8641=PRODUCT('Part 1','Part 1','Part 1',(#8665));
#8642=PRODUCT('Part 1','Part 1','Part 1',(#8666));
#8643=PRODUCT('Part 2','Part 2','Part 2',(#8667));
#8644=PRODUCT('Part 1','Part 1','Part 1',(#8668));
#8645=PRODUCT('Part 4','Part 4','Part 4',(#8669));
#8646=PRODUCT('Part 2','Part 2','Part 2',(#8670));
#8647=PRODUCT('CRANKSHAFT','CRANKSHAFT','CRANKSHAFT',(#8671));
#8648=PRODUCT('Part 3','Part 3','Part 3',(#8672));
#8649=PRODUCT_CATEGORY('','');
#8650=PRODUCT_CATEGORY('','');
#8651=PRODUCT_CATEGORY('','');
#8652=PRODUCT_CATEGORY('','');
#8653=PRODUCT_CATEGORY('','');
#8654=PRODUCT_CATEGORY('','');
#8655=PRODUCT_CATEGORY('','');
#8656=PRODUCT_CATEGORY('','');
#8657=PRODUCT_CATEGORY('','');
#8658=PRODUCT_CATEGORY('','');
#8659=PRODUCT_CATEGORY('','');
#8660=PRODUCT_CATEGORY('','');
#8661=PRODUCT_CONTEXT('',#8674,'mechanical');
#8662=PRODUCT_CONTEXT('',#8674,'mechanical');
#8663=PRODUCT_CONTEXT('',#8674,'mechanical');
#8664=PRODUCT_CONTEXT('',#8674,'mechanical');
#8665=PRODUCT_CONTEXT('',#8674,'mechanical');
#8666=PRODUCT_CONTEXT('',#8674,'mechanical');
#8667=PRODUCT_CONTEXT('',#8674,'mechanical');
#8668=PRODUCT_CONTEXT('',#8674,'mechanical');
#8669=PRODUCT_CONTEXT('',#8674,'mechanical');
#8670=PRODUCT_CONTEXT('',#8674,'mechanical');
#8671=PRODUCT_CONTEXT('',#8674,'mechanical');
#8672=PRODUCT_CONTEXT('',#8674,'mechanical');
#8673=APPLICATION_PROTOCOL_DEFINITION('international standard',
'ap242_managed_model_based_3d_engineering',2020,#8674);
#8674=APPLICATION_CONTEXT('managed model based 3d engineering');
ENDSEC;
END-ISO-10303-21;
